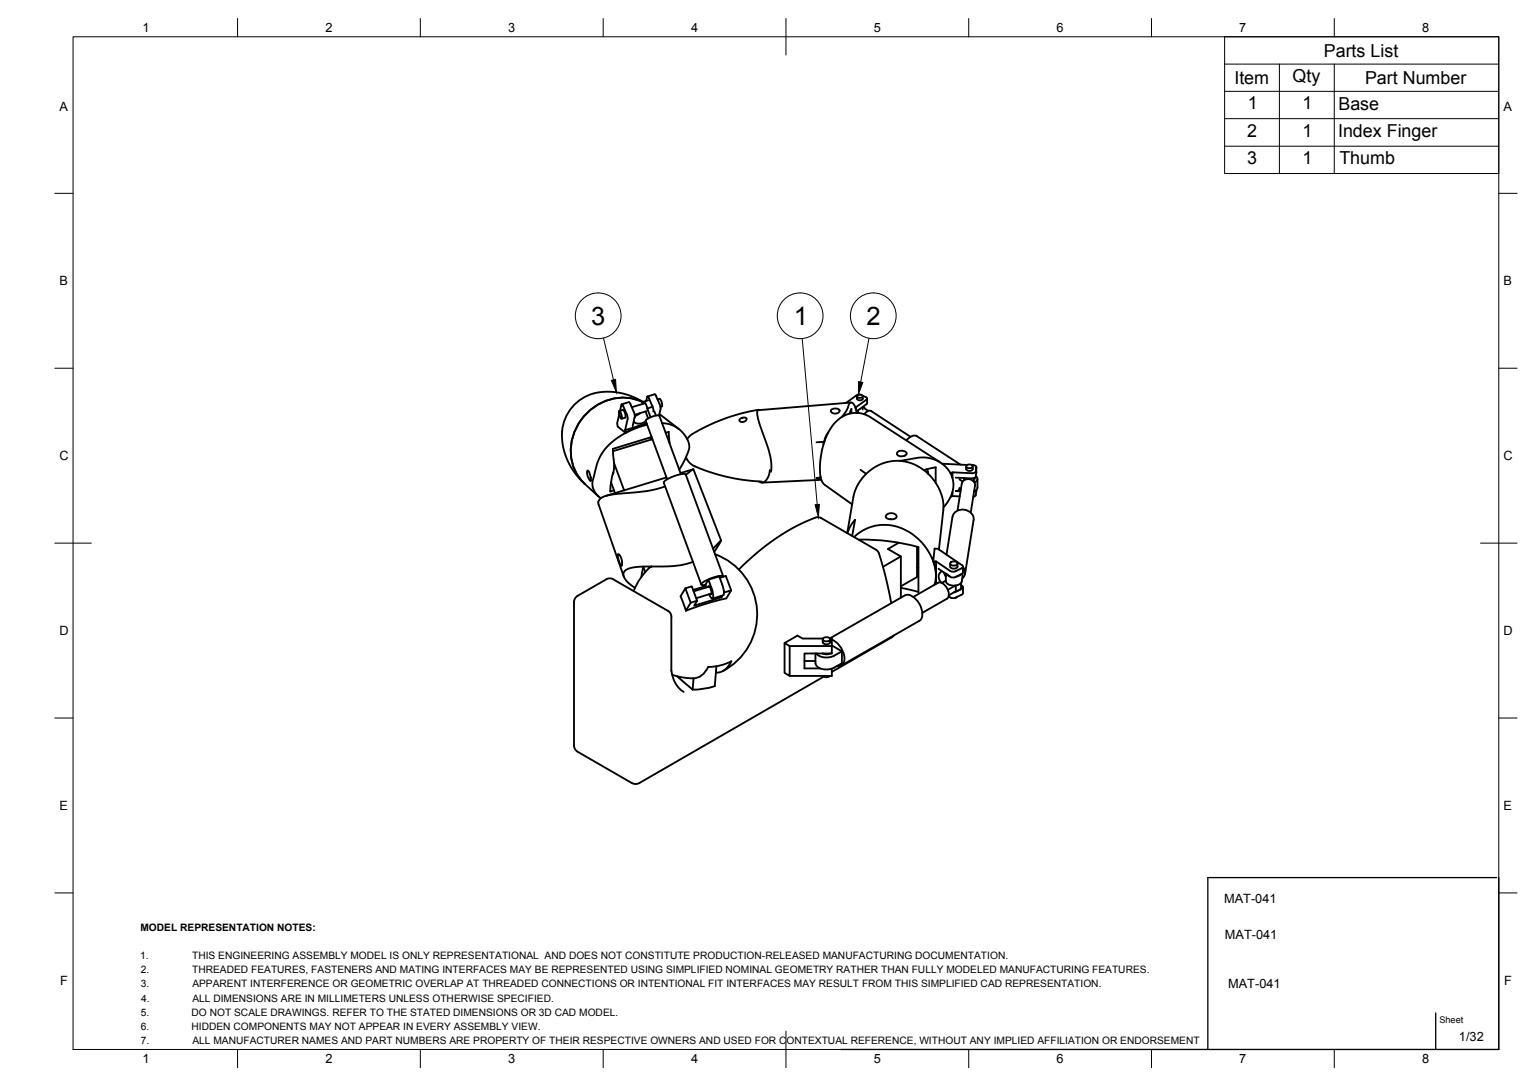
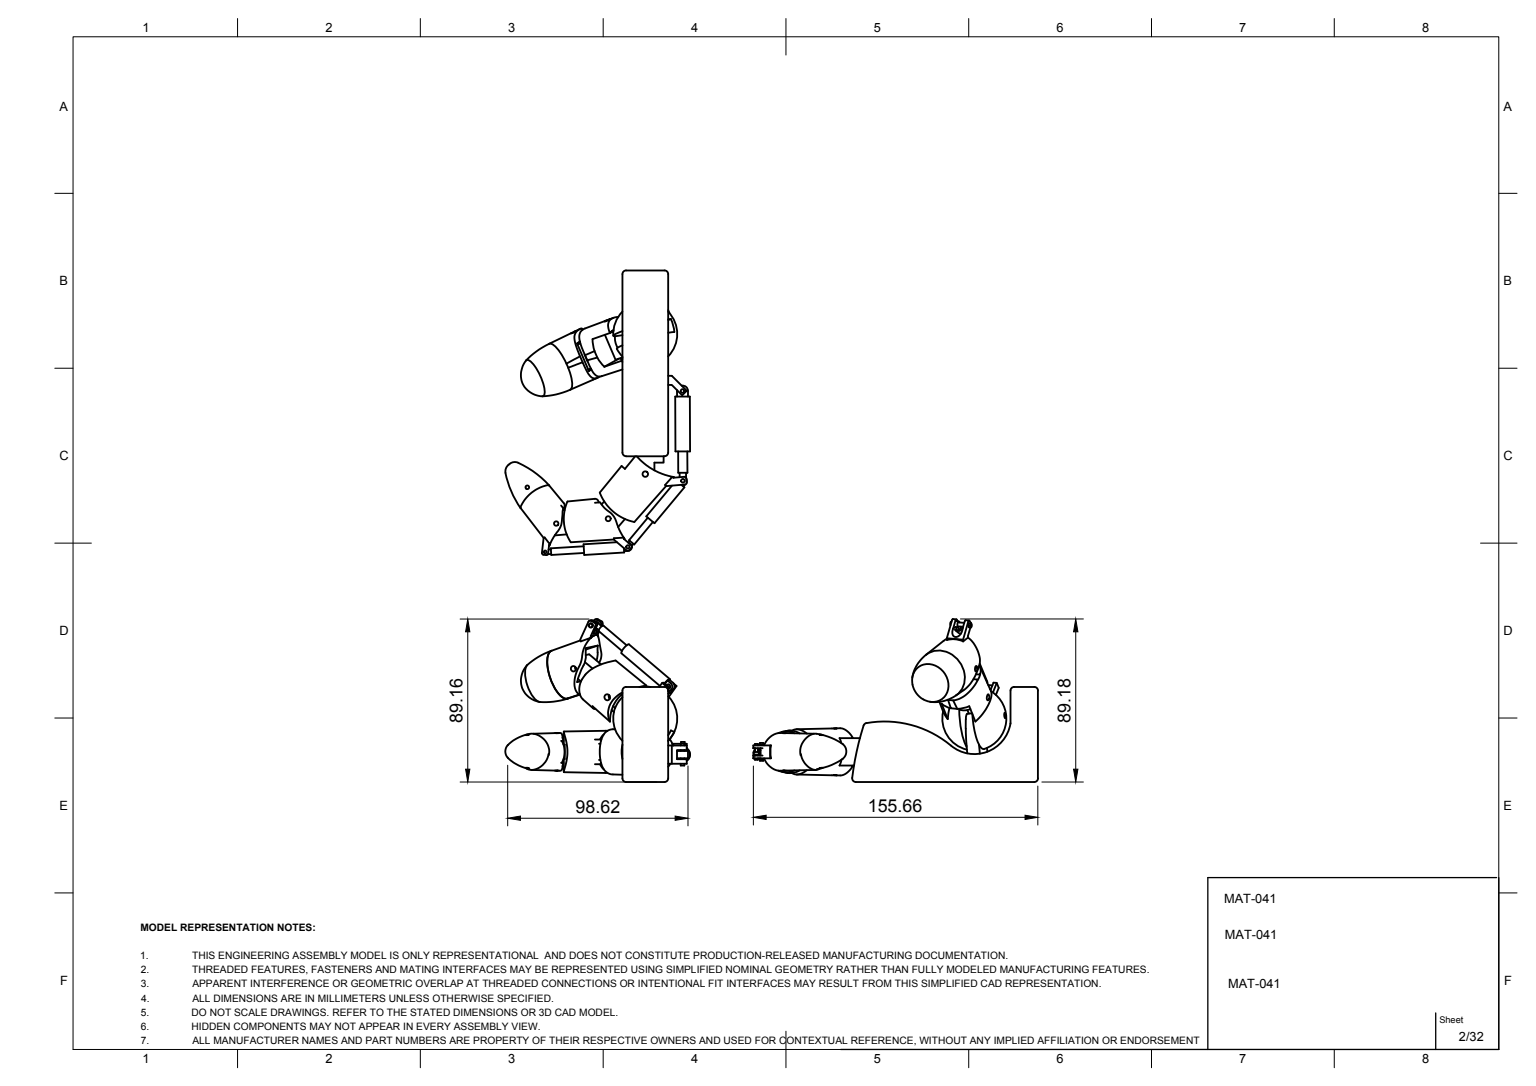
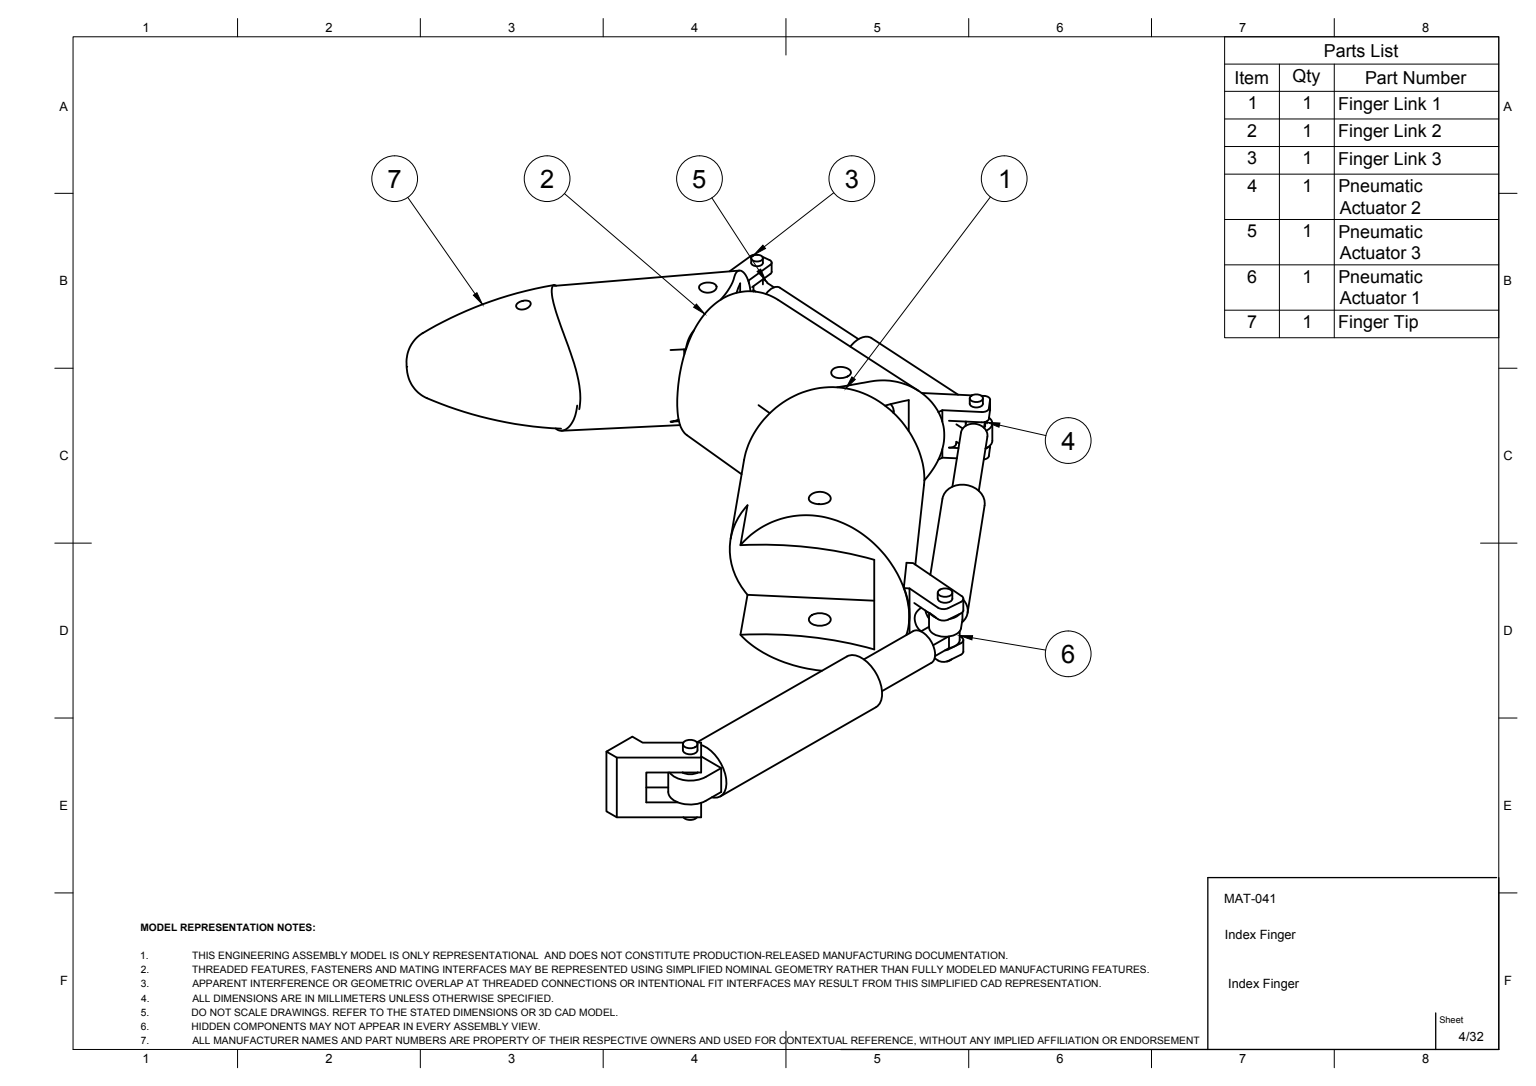
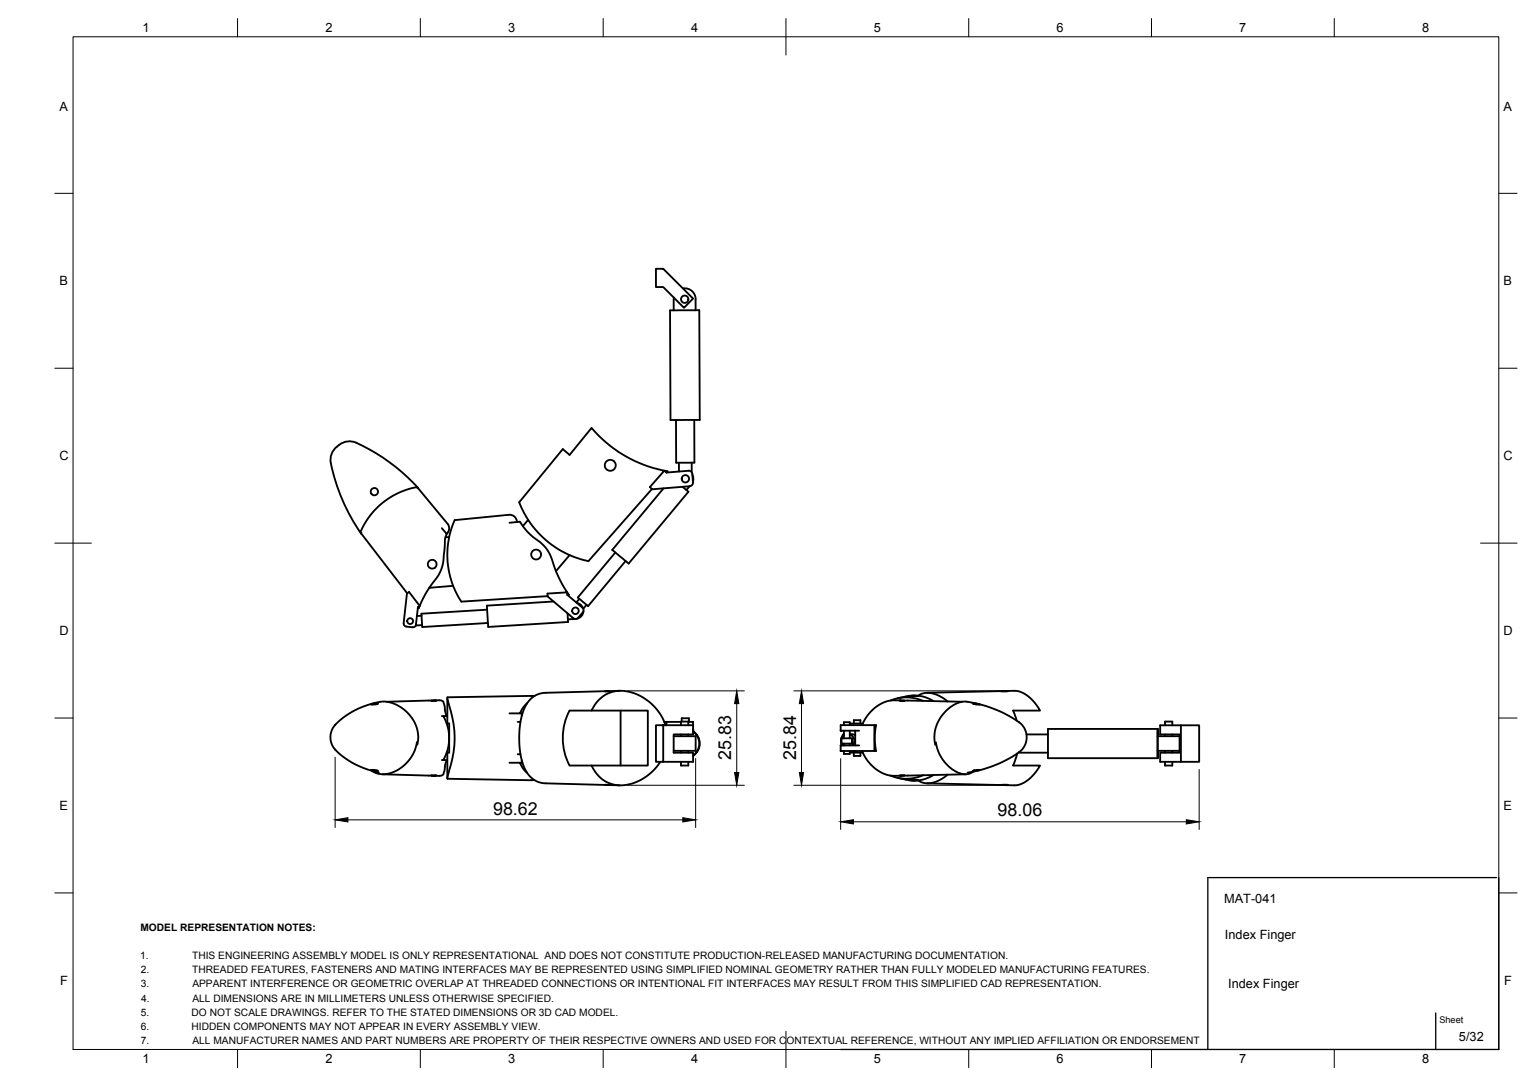
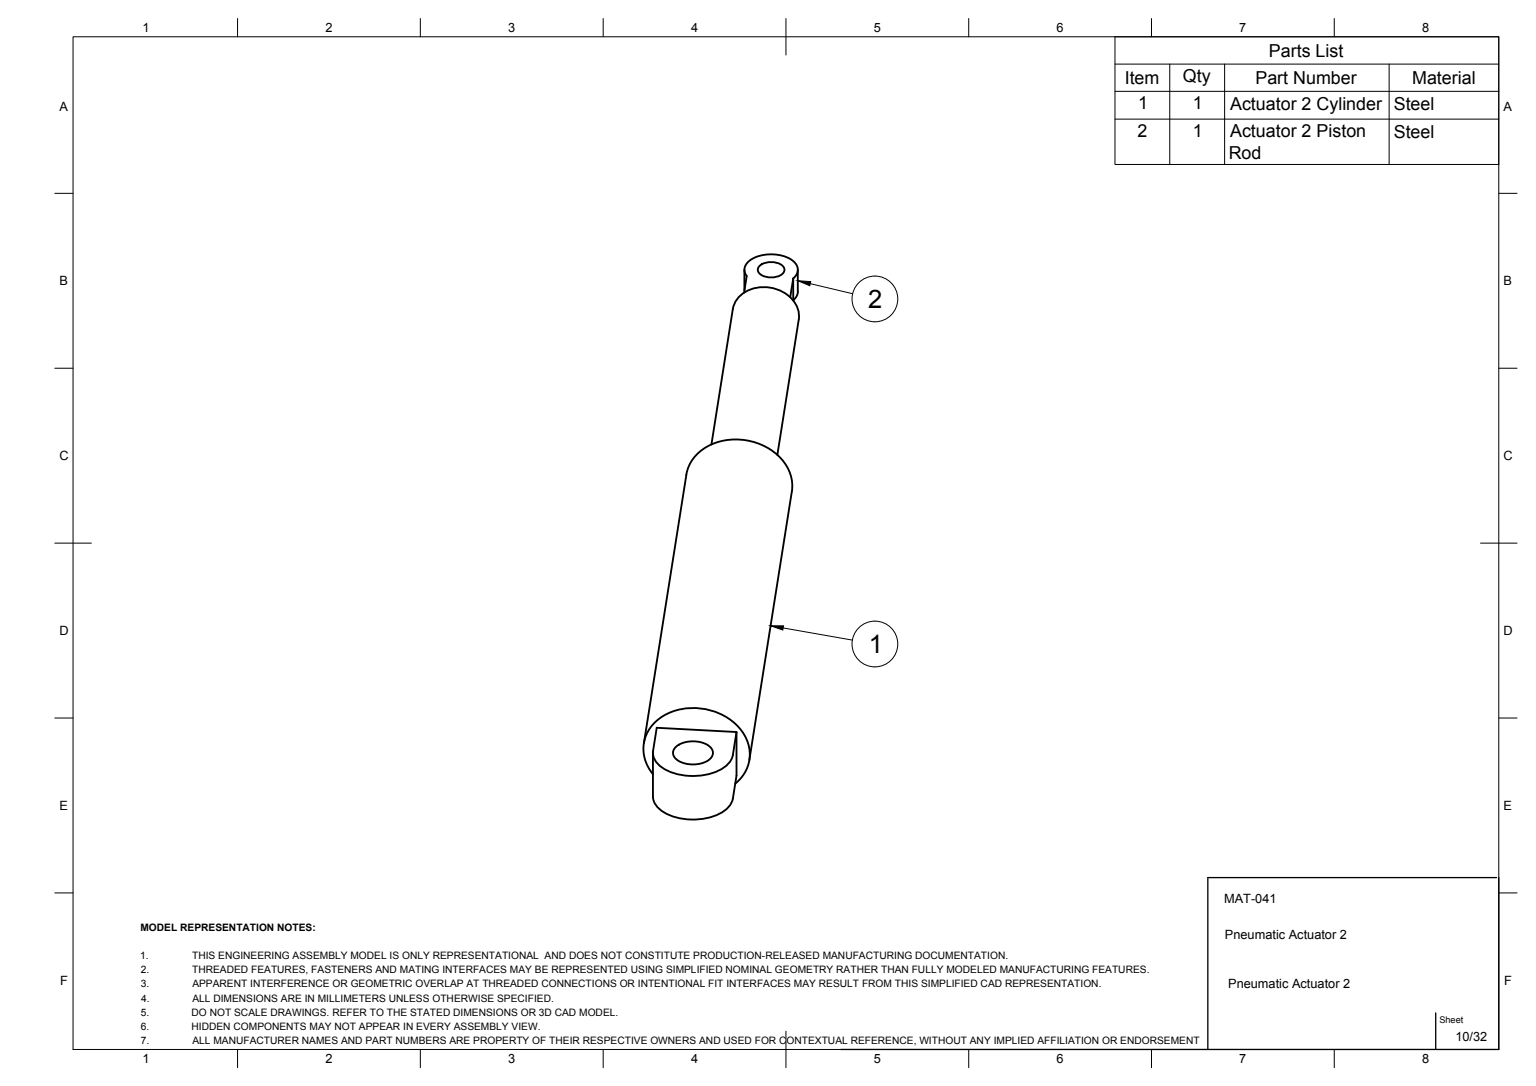
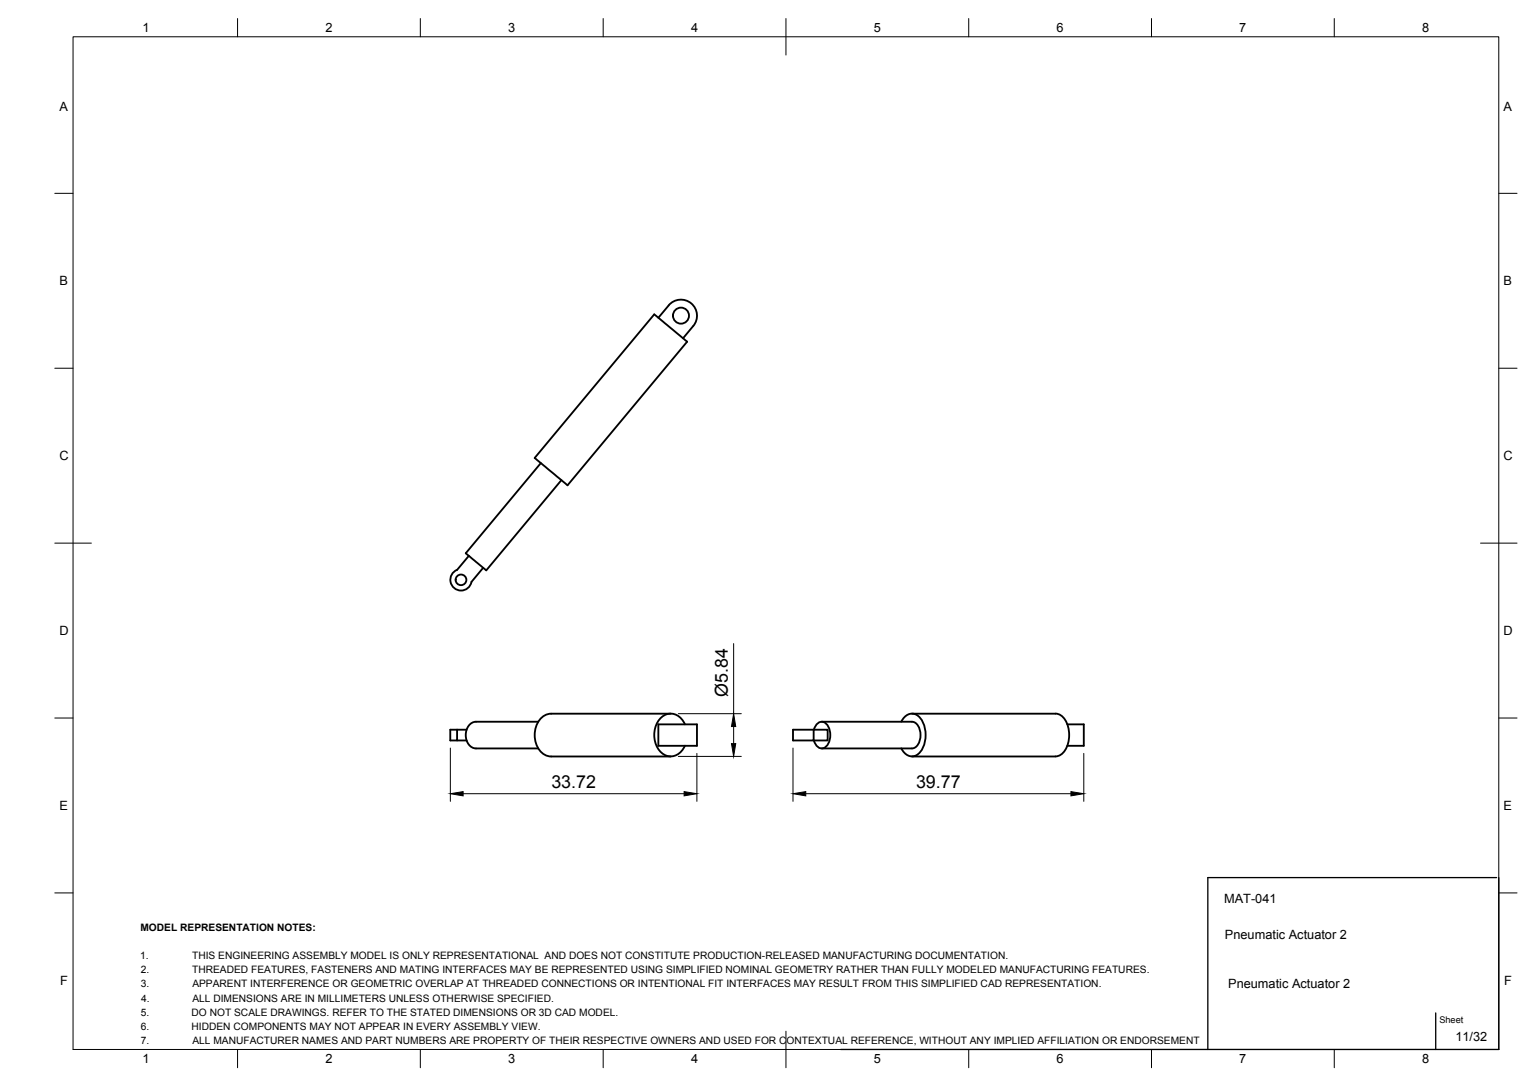
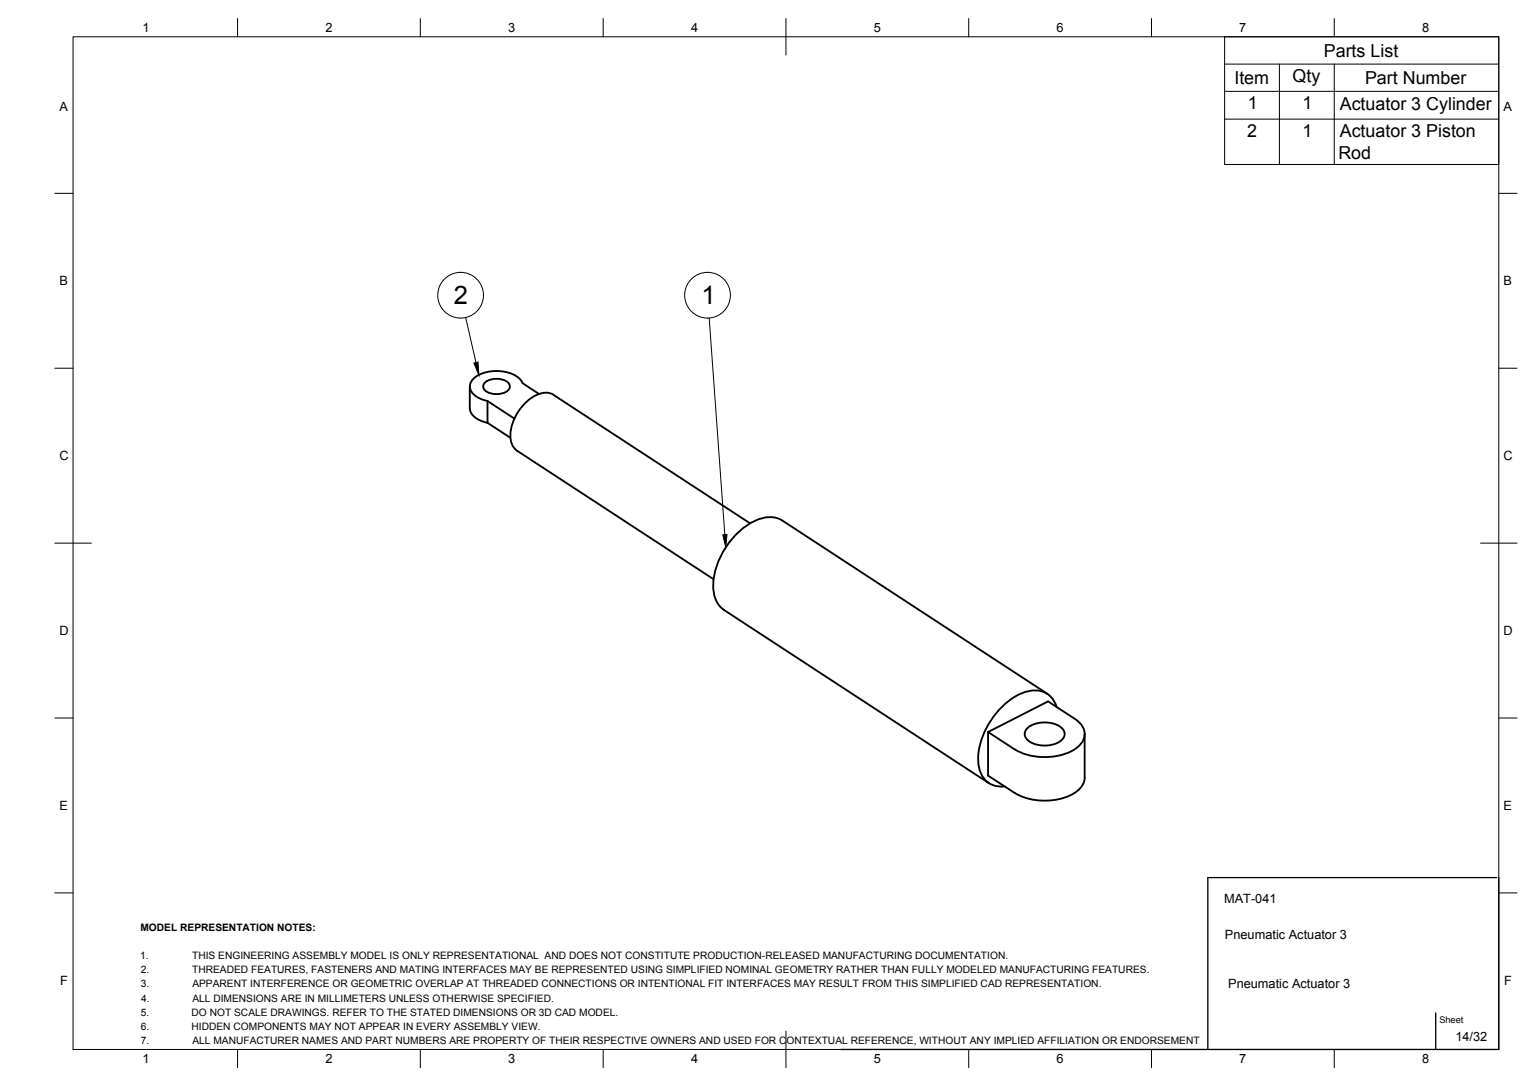
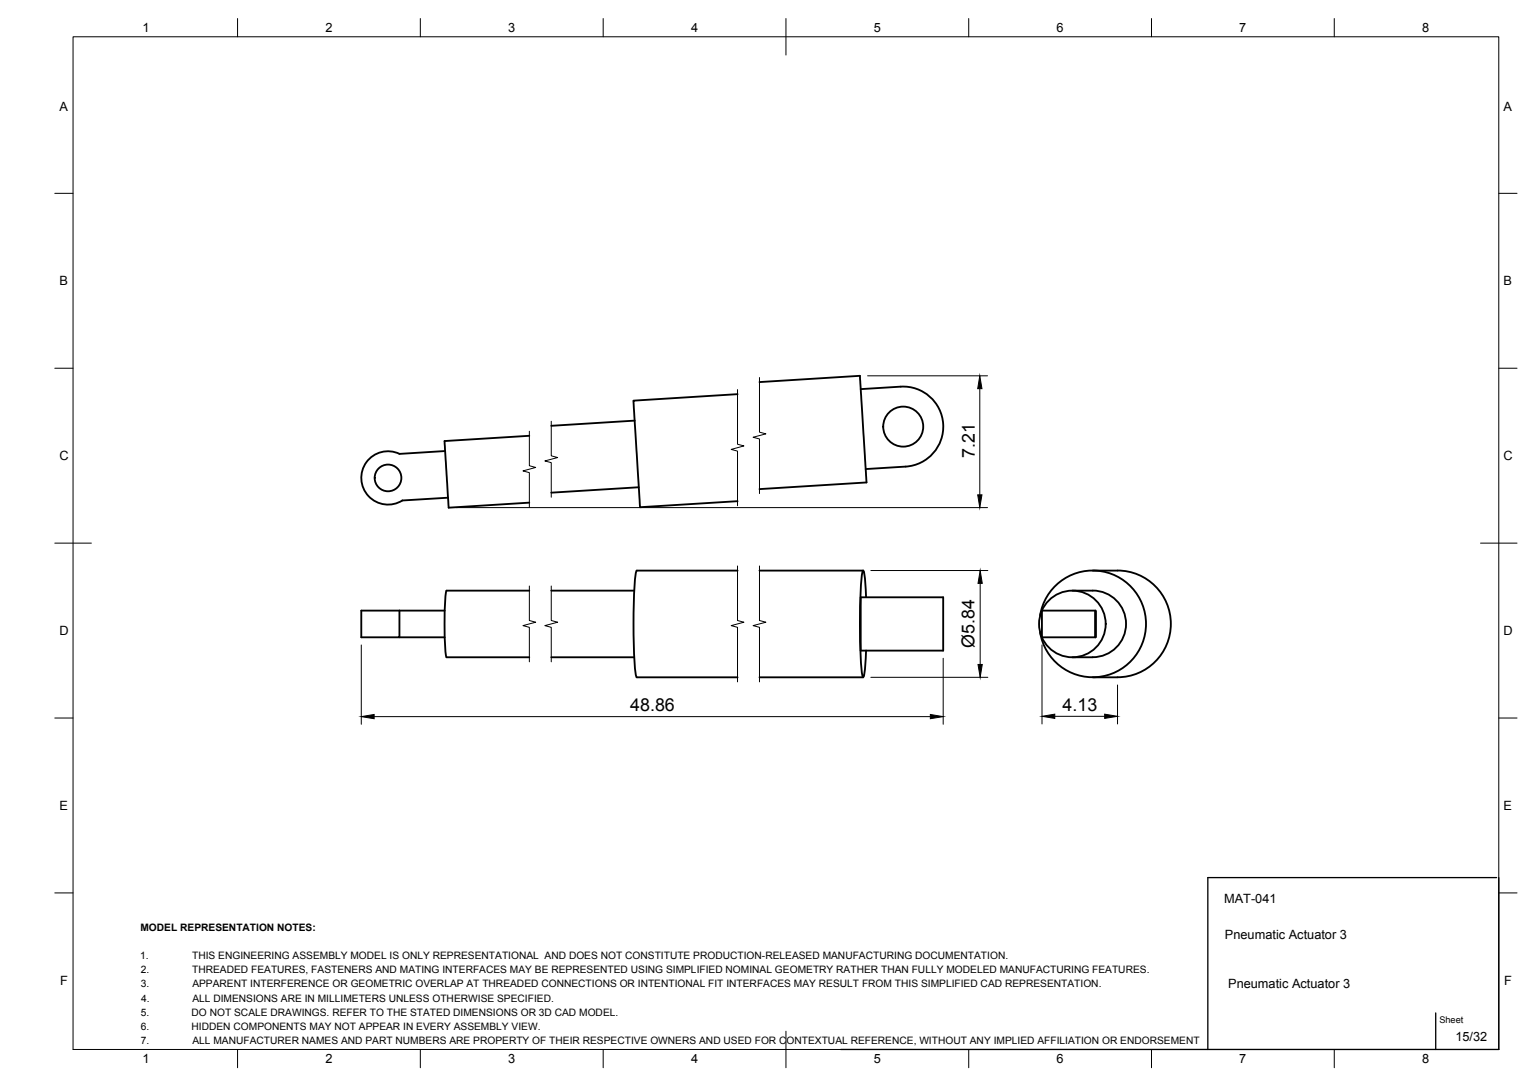
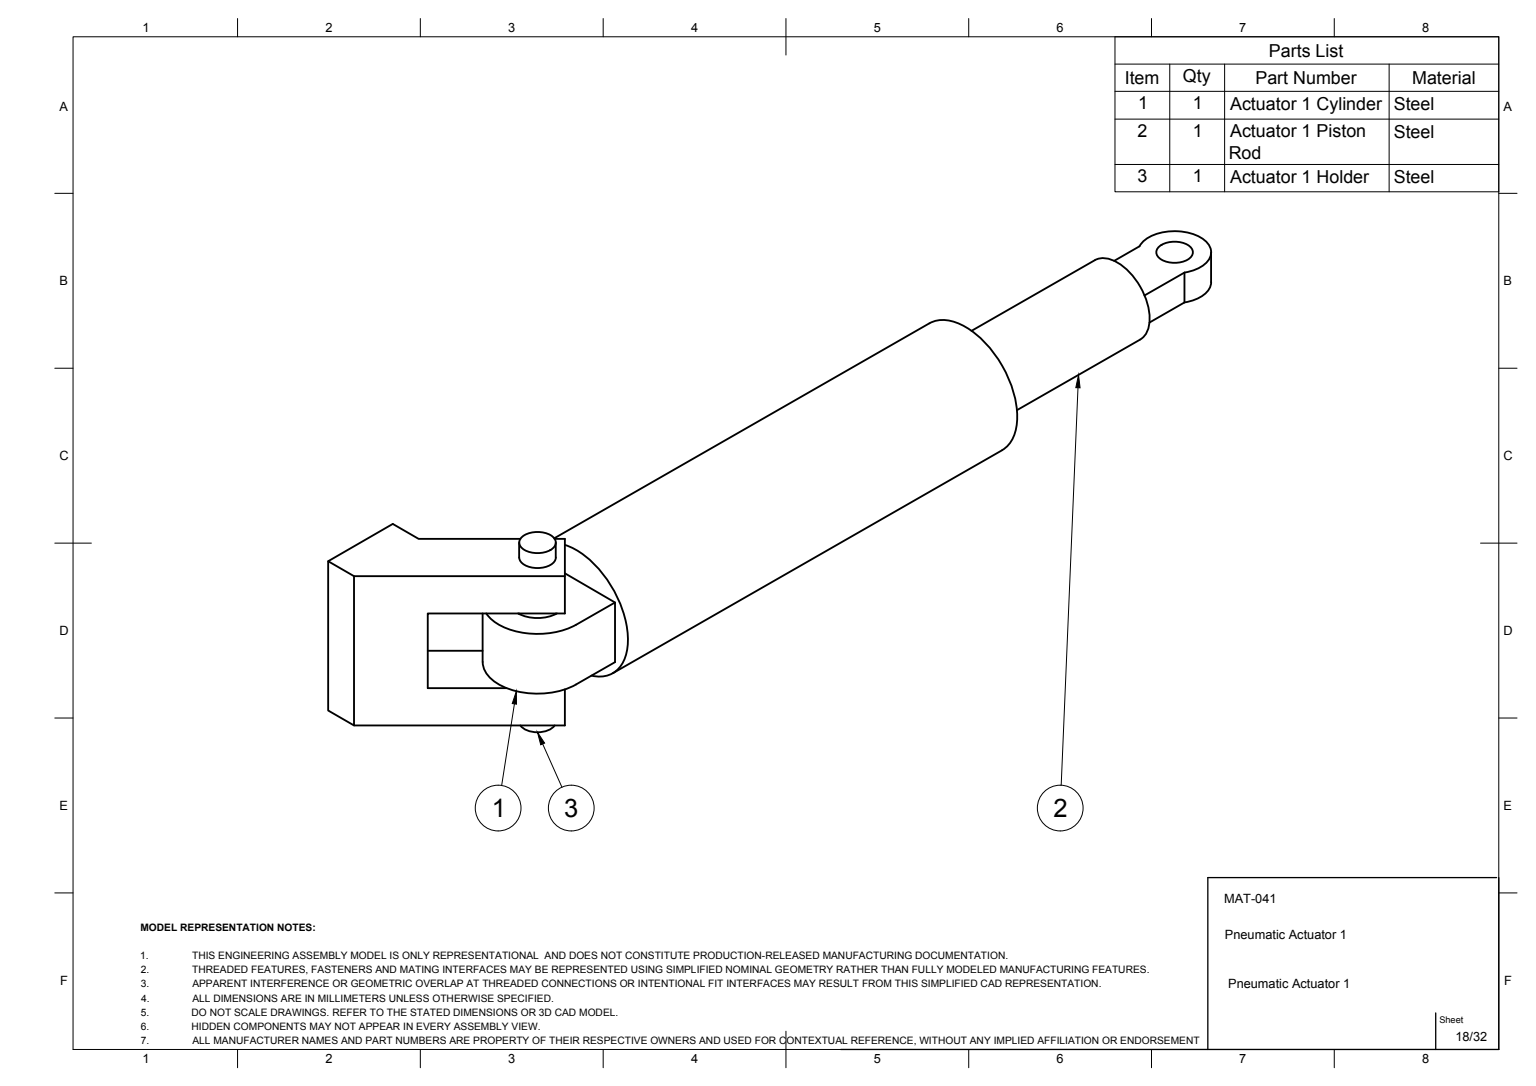
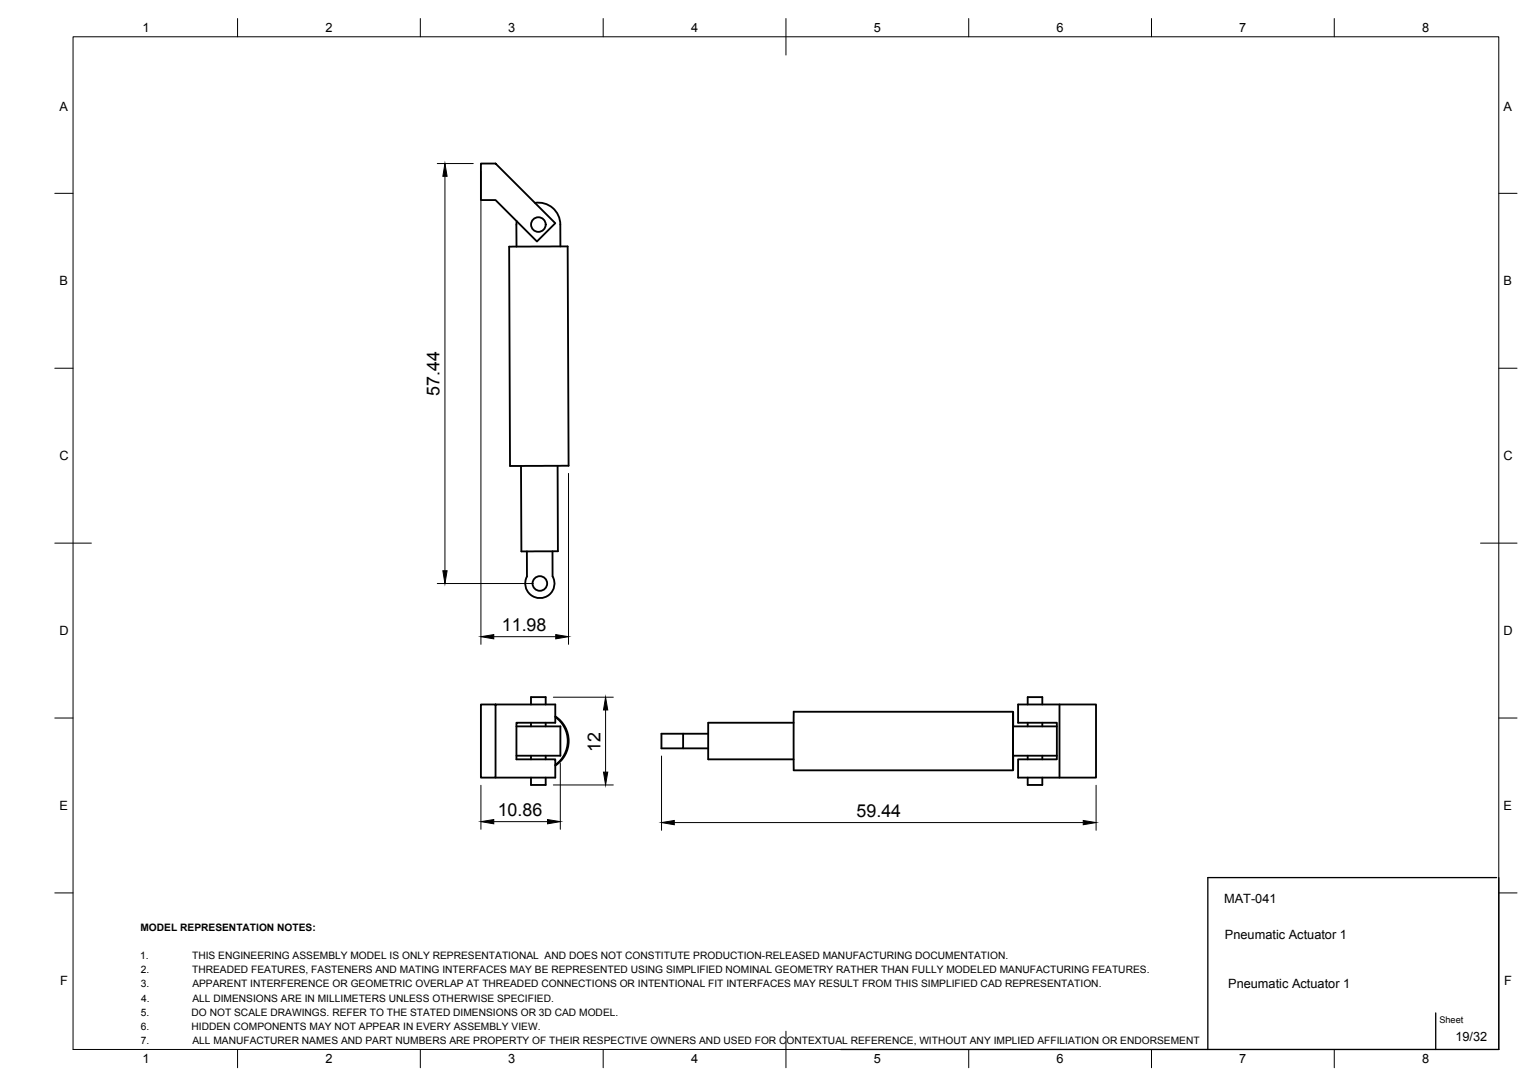
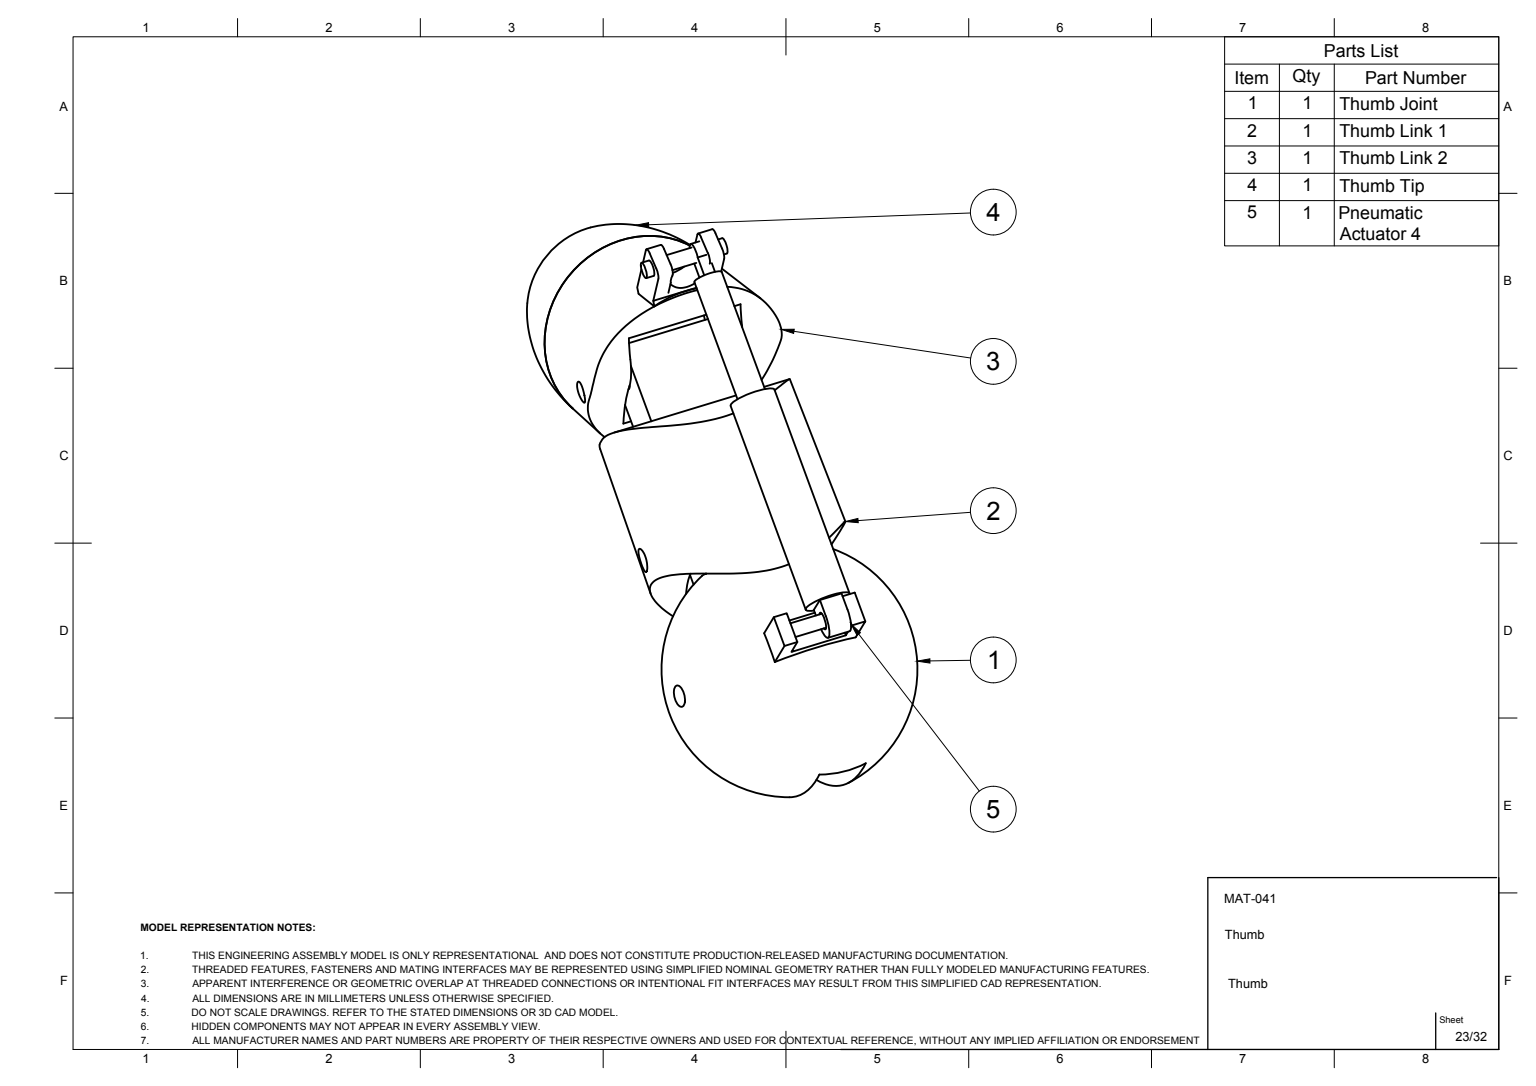
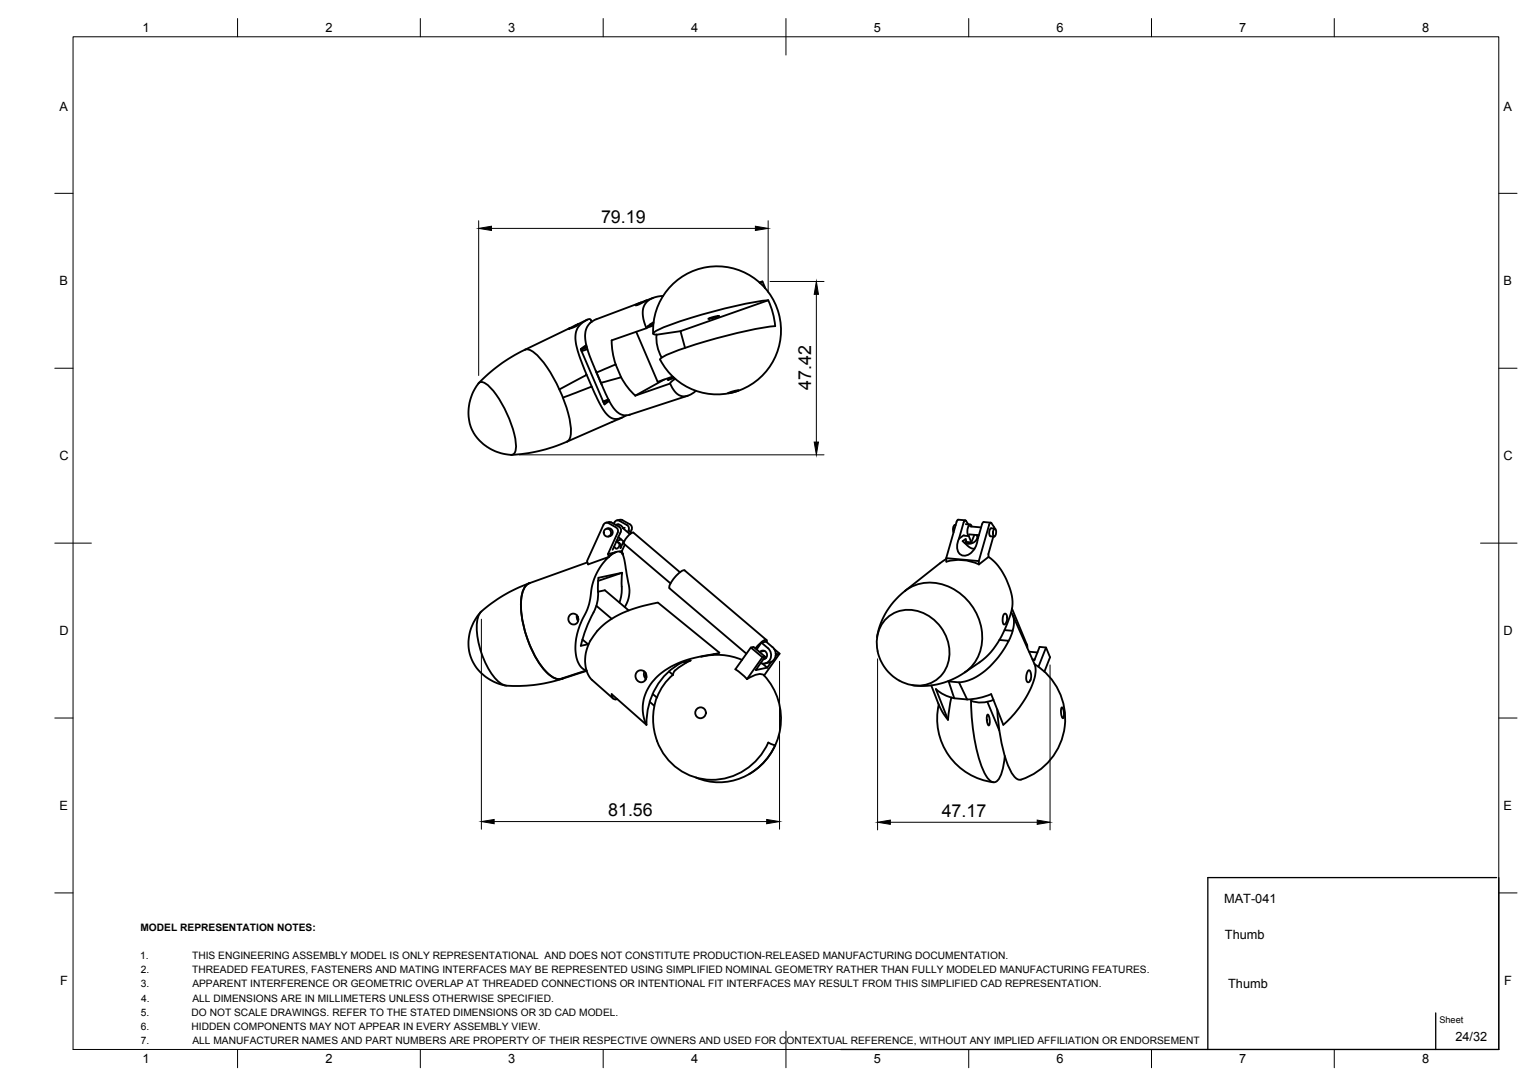
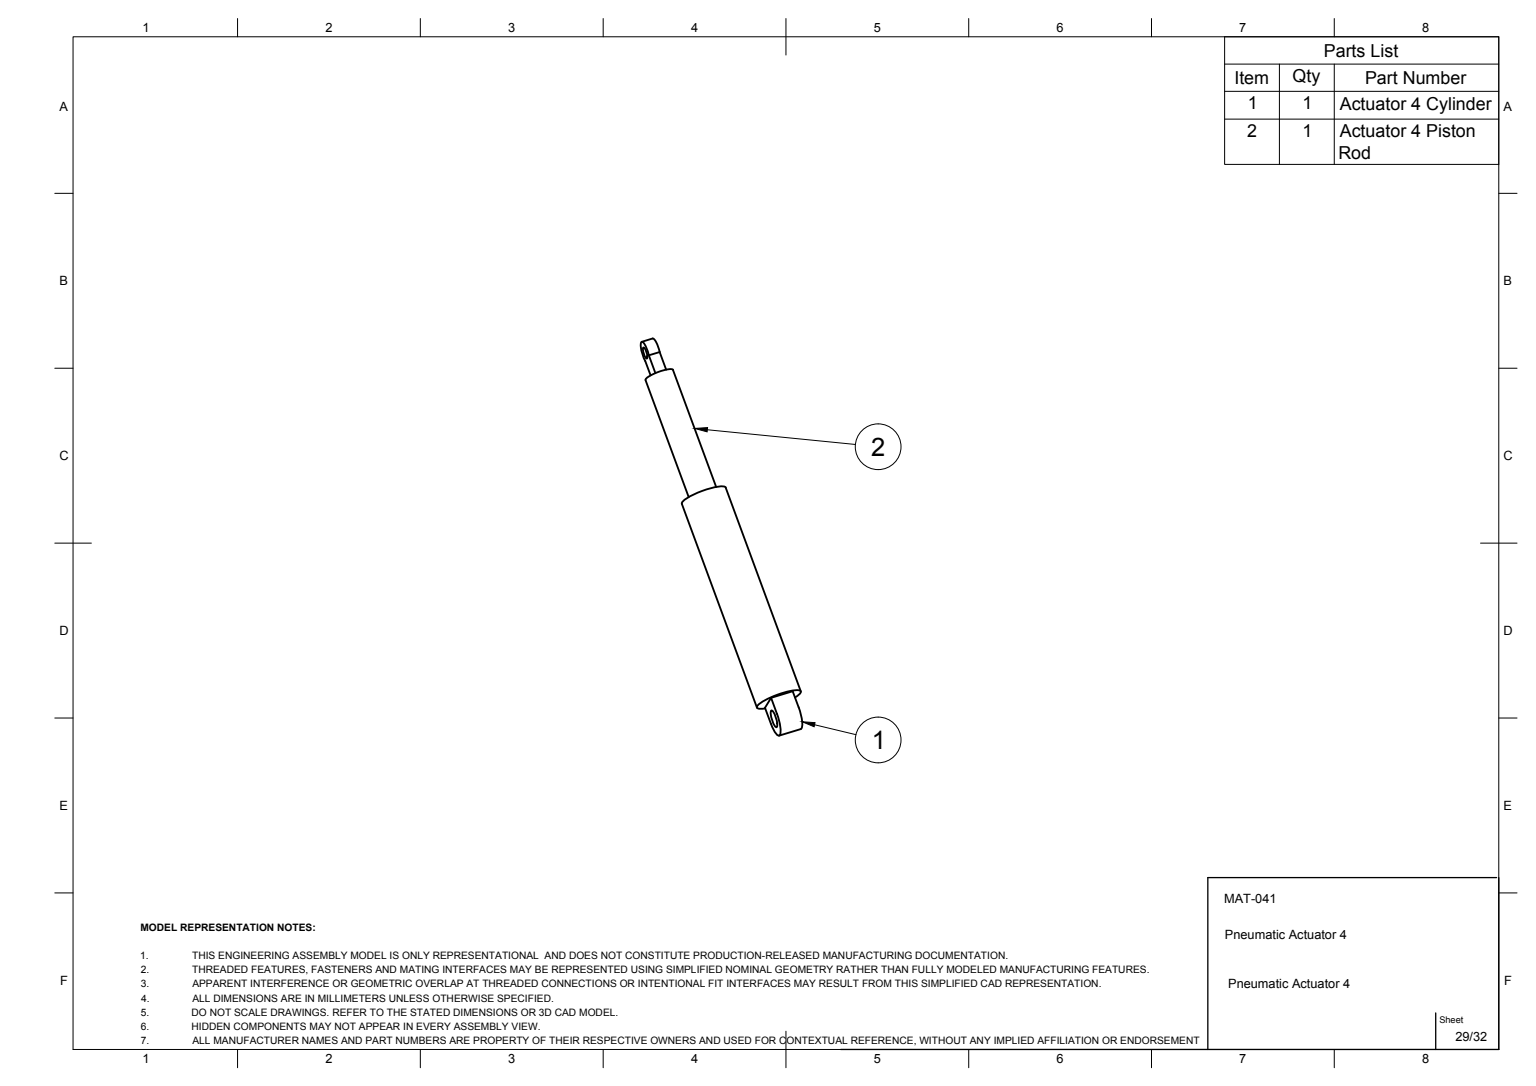
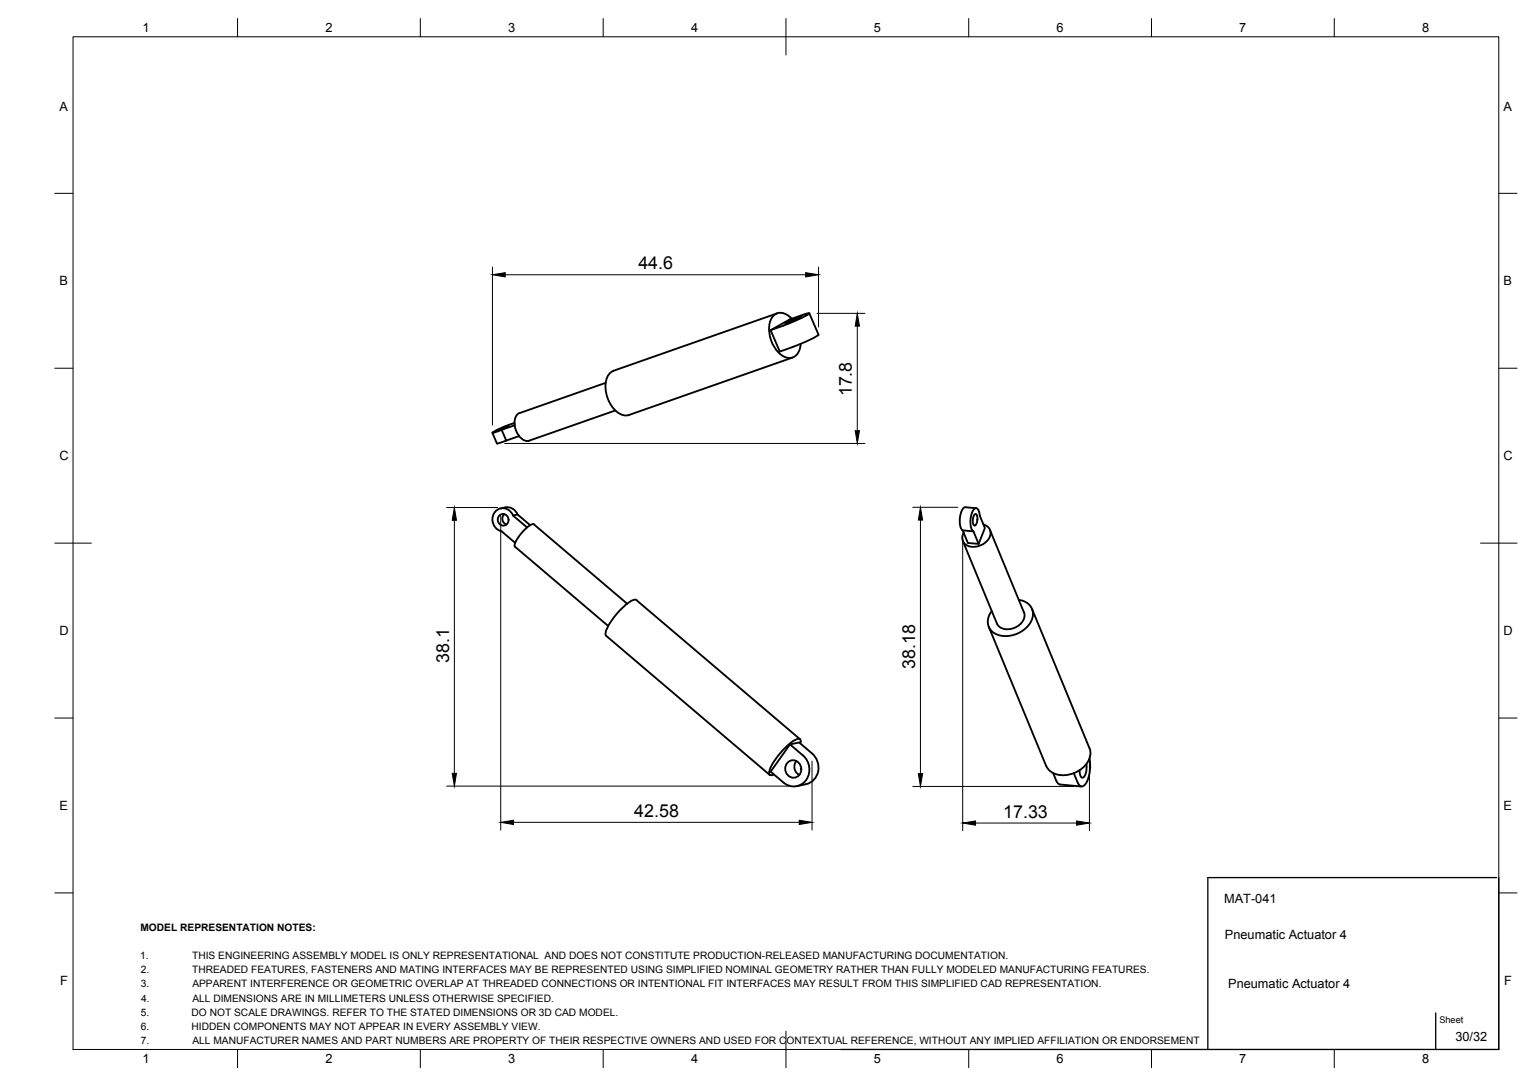
ISO-10303-21;
HEADER;
/* Generated by software containing ST-Developer
 * from STEP Tools, Inc. (www.steptools.com) 
 */

FILE_DESCRIPTION(
/* description */ ('STEP AP214'),
/* implementation_level */ '2;1');

FILE_NAME(
/* name */ 'MAT-041.step',
/* time_stamp */ '2026-11-14T21:57:47-08:00',
/* author */ (''),
/* organization */ (''),
/* preprocessor_version */ 'ST-DEVELOPER v20.2',
/* originating_system */ 'Autodesk Translation Framework v15.17.0.0',
/* authorisation */ '');

FILE_SCHEMA (('AUTOMOTIVE_DESIGN { 1 0 10303 214 3 1 1 }'));
ENDSEC;

DATA;
#10=MECHANICAL_DESIGN_GEOMETRIC_PRESENTATION_REPRESENTATION('',(#248,#249,
#250,#251,#252,#253,#254,#255,#256,#257,#258,#259,#260,#261,#262,#263,#264,
#265),#13199);
#11=(
BOUNDED_CURVE()
B_SPLINE_CURVE(2,(#12139,#12140,#12141),.UNSPECIFIED.,.F.,.F.)
B_SPLINE_CURVE_WITH_KNOTS((3,3),(0.0658194535624849,0.468554524158603),
 .UNSPECIFIED.)
CURVE()
GEOMETRIC_REPRESENTATION_ITEM()
RATIONAL_B_SPLINE_CURVE((0.999935484054137,0.979761934520674,1.))
REPRESENTATION_ITEM('')
);
#12=(
BOUNDED_CURVE()
B_SPLINE_CURVE(2,(#12481,#12482,#12483),.UNSPECIFIED.,.F.,.F.)
B_SPLINE_CURVE_WITH_KNOTS((3,3),(-1.60124615225297,-0.808783730274253),
 .UNSPECIFIED.)
CURVE()
GEOMETRIC_REPRESENTATION_ITEM()
RATIONAL_B_SPLINE_CURVE((1.00284139361103,1.00297035013721,1.00227572336188))
REPRESENTATION_ITEM('')
);
#13=(
BOUNDED_CURVE()
B_SPLINE_CURVE(2,(#12547,#12548,#12549),.UNSPECIFIED.,.F.,.F.)
B_SPLINE_CURVE_WITH_KNOTS((3,3),(-2.14592066681242,-1.35342729440919),
 .UNSPECIFIED.)
CURVE()
GEOMETRIC_REPRESENTATION_ITEM()
RATIONAL_B_SPLINE_CURVE((1.00227603694351,1.00297081766941,1.00284201479666))
REPRESENTATION_ITEM('')
);
#14=(
BOUNDED_CURVE()
B_SPLINE_CURVE(2,(#12779,#12780,#12781),.UNSPECIFIED.,.F.,.F.)
B_SPLINE_CURVE_WITH_KNOTS((3,3),(-2.71364129597392,-1.62020359036119),
 .UNSPECIFIED.)
CURVE()
GEOMETRIC_REPRESENTATION_ITEM()
RATIONAL_B_SPLINE_CURVE((1.0005626059293,1.00242625759818,1.00269667985146))
REPRESENTATION_ITEM('')
);
#15=(
BOUNDED_CURVE()
B_SPLINE_CURVE(2,(#12785,#12786,#12787),.UNSPECIFIED.,.F.,.F.)
B_SPLINE_CURVE_WITH_KNOTS((3,3),(-1.2490205262323,-0.155582820602816),
 .UNSPECIFIED.)
CURVE()
GEOMETRIC_REPRESENTATION_ITEM()
RATIONAL_B_SPLINE_CURVE((1.00269667985147,1.00242625759819,1.00056260592924))
REPRESENTATION_ITEM('')
);
#16=(
BOUNDED_CURVE()
B_SPLINE_CURVE(2,(#12826,#12827,#12828),.UNSPECIFIED.,.F.,.F.)
B_SPLINE_CURVE_WITH_KNOTS((3,3),(0.587541837462245,1.2406747936684),
 .UNSPECIFIED.)
CURVE()
GEOMETRIC_REPRESENTATION_ITEM()
RATIONAL_B_SPLINE_CURVE((1.00007054095476,1.00010145473128,1.00011392829506))
REPRESENTATION_ITEM('')
);
#17=(
BOUNDED_SURFACE()
B_SPLINE_SURFACE(2,2,((#12039,#12040,#12041,#12042,#12043,#12044,#12045,
#12046,#12047),(#12048,#12049,#12050,#12051,#12052,#12053,#12054,#12055,
#12056),(#12057,#12058,#12059,#12060,#12061,#12062,#12063,#12064,#12065)),
 .UNSPECIFIED.,.F.,.T.,.F.)
B_SPLINE_SURFACE_WITH_KNOTS((3,3),(3,2,2,2,3),(-1.66348996389916,-0.482485072527983),
(-3.14159265358979,-1.5707963267949,0.,1.5707963267949,3.14159265358979),
 .UNSPECIFIED.)
GEOMETRIC_REPRESENTATION_ITEM()
RATIONAL_B_SPLINE_SURFACE(((1.,0.707106781186548,1.,0.707106781186548,1.,
0.707106781186548,1.,0.707106781186548,1.),(0.830661033030149,0.587366049323041,
0.830661033030149,0.587366049323041,0.830661033030149,0.587366049323041,
0.830661033030149,0.587366049323041,0.830661033030149),(1.,0.707106781186548,
1.,0.707106781186548,1.,0.707106781186548,1.,0.707106781186548,1.)))
REPRESENTATION_ITEM('')
SURFACE()
);
#18=(
BOUNDED_SURFACE()
B_SPLINE_SURFACE(2,2,((#12070,#12071,#12072,#12073,#12074,#12075,#12076,
#12077,#12078),(#12079,#12080,#12081,#12082,#12083,#12084,#12085,#12086,
#12087),(#12088,#12089,#12090,#12091,#12092,#12093,#12094,#12095,#12096)),
 .UNSPECIFIED.,.F.,.T.,.F.)
B_SPLINE_SURFACE_WITH_KNOTS((3,3),(3,2,2,2,3),(-0.468554524158603,-0.0651764989564067),
(-3.14159265358979,-1.5707963267949,0.,1.5707963267949,3.14159265358979),
 .UNSPECIFIED.)
GEOMETRIC_REPRESENTATION_ITEM()
RATIONAL_B_SPLINE_SURFACE(((1.,0.707106781186548,1.,0.707106781186548,1.,
0.707106781186548,1.,0.707106781186548,1.),(0.979729625048845,0.692773461601392,
0.979729625048845,0.692773461601392,0.979729625048845,0.692773461601392,
0.979729625048845,0.692773461601392,0.979729625048845),(1.,0.707106781186548,
1.,0.707106781186548,1.,0.707106781186548,1.,0.707106781186548,1.)))
REPRESENTATION_ITEM('')
SURFACE()
);
#19=(
BOUNDED_SURFACE()
B_SPLINE_SURFACE(2,2,((#12988,#12989,#12990,#12991,#12992,#12993,#12994,
#12995,#12996),(#12997,#12998,#12999,#13000,#13001,#13002,#13003,#13004,
#13005),(#13006,#13007,#13008,#13009,#13010,#13011,#13012,#13013,#13014)),
 .UNSPECIFIED.,.F.,.T.,.F.)
B_SPLINE_SURFACE_WITH_KNOTS((3,3),(3,2,2,2,3),(-1.48074001480244,-0.468405301545521),
(-3.14159265358979,-1.5707963267949,0.,1.5707963267949,3.14159265358979),
 .UNSPECIFIED.)
GEOMETRIC_REPRESENTATION_ITEM()
RATIONAL_B_SPLINE_SURFACE(((1.,0.707106781186548,1.,0.707106781186548,1.,
0.707106781186548,1.,0.707106781186548,1.),(0.874609102422644,0.618442027210531,
0.874609102422644,0.618442027210531,0.874609102422644,0.618442027210531,
0.874609102422644,0.618442027210531,0.874609102422644),(1.,0.707106781186548,
1.,0.707106781186548,1.,0.707106781186548,1.,0.707106781186548,1.)))
REPRESENTATION_ITEM('')
SURFACE()
);
#20=(
BOUNDED_SURFACE()
B_SPLINE_SURFACE(2,2,((#13019,#13020,#13021,#13022,#13023,#13024,#13025,
#13026,#13027),(#13028,#13029,#13030,#13031,#13032,#13033,#13034,#13035,
#13036),(#13037,#13038,#13039,#13040,#13041,#13042,#13043,#13044,#13045)),
 .UNSPECIFIED.,.F.,.T.,.F.)
B_SPLINE_SURFACE_WITH_KNOTS((3,3),(3,2,2,2,3),(-0.359971068140638,-0.0153537783592699),
(-3.14159265358979,-1.5707963267949,0.,1.5707963267949,3.14159265358979),
 .UNSPECIFIED.)
GEOMETRIC_REPRESENTATION_ITEM()
RATIONAL_B_SPLINE_SURFACE(((1.,0.707106781186548,1.,0.707106781186548,1.,
0.707106781186548,1.,0.707106781186548,1.),(0.985191558786762,0.696635631985865,
0.985191558786762,0.696635631985865,0.985191558786762,0.696635631985865,
0.985191558786762,0.696635631985865,0.985191558786762),(1.,0.707106781186548,
1.,0.707106781186548,1.,0.707106781186548,1.,0.707106781186548,1.)))
REPRESENTATION_ITEM('')
SURFACE()
);
#21=ITEM_DEFINED_TRANSFORMATION($,$,#7454,#7490);
#22=ITEM_DEFINED_TRANSFORMATION($,$,#7474,#7491);
#23=ITEM_DEFINED_TRANSFORMATION($,$,#7493,#7529);
#24=ITEM_DEFINED_TRANSFORMATION($,$,#7513,#7530);
#25=ITEM_DEFINED_TRANSFORMATION($,$,#7532,#7592);
#26=ITEM_DEFINED_TRANSFORMATION($,$,#7552,#7593);
#27=ITEM_DEFINED_TRANSFORMATION($,$,#7568,#7594);
#28=ITEM_DEFINED_TRANSFORMATION($,$,#7193,#7610);
#29=ITEM_DEFINED_TRANSFORMATION($,$,#7274,#7611);
#30=ITEM_DEFINED_TRANSFORMATION($,$,#7359,#7612);
#31=ITEM_DEFINED_TRANSFORMATION($,$,#7453,#7613);
#32=ITEM_DEFINED_TRANSFORMATION($,$,#7492,#7614);
#33=ITEM_DEFINED_TRANSFORMATION($,$,#7531,#7615);
#34=ITEM_DEFINED_TRANSFORMATION($,$,#7595,#7616);
#35=ITEM_DEFINED_TRANSFORMATION($,$,#7783,#7819);
#36=ITEM_DEFINED_TRANSFORMATION($,$,#7803,#7820);
#37=ITEM_DEFINED_TRANSFORMATION($,$,#7618,#7821);
#38=ITEM_DEFINED_TRANSFORMATION($,$,#7666,#7822);
#39=ITEM_DEFINED_TRANSFORMATION($,$,#7700,#7823);
#40=ITEM_DEFINED_TRANSFORMATION($,$,#7776,#7824);
#41=ITEM_DEFINED_TRANSFORMATION($,$,#7782,#7825);
#42=ITEM_DEFINED_TRANSFORMATION($,$,#7061,#7826);
#43=ITEM_DEFINED_TRANSFORMATION($,$,#7192,#7827);
#44=ITEM_DEFINED_TRANSFORMATION($,$,#7617,#7828);
#45=(
REPRESENTATION_RELATIONSHIP($,$,#13285,#13284)
REPRESENTATION_RELATIONSHIP_WITH_TRANSFORMATION(#21)
SHAPE_REPRESENTATION_RELATIONSHIP()
);
#46=(
REPRESENTATION_RELATIONSHIP($,$,#13286,#13284)
REPRESENTATION_RELATIONSHIP_WITH_TRANSFORMATION(#22)
SHAPE_REPRESENTATION_RELATIONSHIP()
);
#47=(
REPRESENTATION_RELATIONSHIP($,$,#13288,#13287)
REPRESENTATION_RELATIONSHIP_WITH_TRANSFORMATION(#23)
SHAPE_REPRESENTATION_RELATIONSHIP()
);
#48=(
REPRESENTATION_RELATIONSHIP($,$,#13289,#13287)
REPRESENTATION_RELATIONSHIP_WITH_TRANSFORMATION(#24)
SHAPE_REPRESENTATION_RELATIONSHIP()
);
#49=(
REPRESENTATION_RELATIONSHIP($,$,#13291,#13290)
REPRESENTATION_RELATIONSHIP_WITH_TRANSFORMATION(#25)
SHAPE_REPRESENTATION_RELATIONSHIP()
);
#50=(
REPRESENTATION_RELATIONSHIP($,$,#13292,#13290)
REPRESENTATION_RELATIONSHIP_WITH_TRANSFORMATION(#26)
SHAPE_REPRESENTATION_RELATIONSHIP()
);
#51=(
REPRESENTATION_RELATIONSHIP($,$,#13293,#13290)
REPRESENTATION_RELATIONSHIP_WITH_TRANSFORMATION(#27)
SHAPE_REPRESENTATION_RELATIONSHIP()
);
#52=(
REPRESENTATION_RELATIONSHIP($,$,#13281,#13280)
REPRESENTATION_RELATIONSHIP_WITH_TRANSFORMATION(#28)
SHAPE_REPRESENTATION_RELATIONSHIP()
);
#53=(
REPRESENTATION_RELATIONSHIP($,$,#13282,#13280)
REPRESENTATION_RELATIONSHIP_WITH_TRANSFORMATION(#29)
SHAPE_REPRESENTATION_RELATIONSHIP()
);
#54=(
REPRESENTATION_RELATIONSHIP($,$,#13283,#13280)
REPRESENTATION_RELATIONSHIP_WITH_TRANSFORMATION(#30)
SHAPE_REPRESENTATION_RELATIONSHIP()
);
#55=(
REPRESENTATION_RELATIONSHIP($,$,#13284,#13280)
REPRESENTATION_RELATIONSHIP_WITH_TRANSFORMATION(#31)
SHAPE_REPRESENTATION_RELATIONSHIP()
);
#56=(
REPRESENTATION_RELATIONSHIP($,$,#13287,#13280)
REPRESENTATION_RELATIONSHIP_WITH_TRANSFORMATION(#32)
SHAPE_REPRESENTATION_RELATIONSHIP()
);
#57=(
REPRESENTATION_RELATIONSHIP($,$,#13290,#13280)
REPRESENTATION_RELATIONSHIP_WITH_TRANSFORMATION(#33)
SHAPE_REPRESENTATION_RELATIONSHIP()
);
#58=(
REPRESENTATION_RELATIONSHIP($,$,#13294,#13280)
REPRESENTATION_RELATIONSHIP_WITH_TRANSFORMATION(#34)
SHAPE_REPRESENTATION_RELATIONSHIP()
);
#59=(
REPRESENTATION_RELATIONSHIP($,$,#13301,#13300)
REPRESENTATION_RELATIONSHIP_WITH_TRANSFORMATION(#35)
SHAPE_REPRESENTATION_RELATIONSHIP()
);
#60=(
REPRESENTATION_RELATIONSHIP($,$,#13302,#13300)
REPRESENTATION_RELATIONSHIP_WITH_TRANSFORMATION(#36)
SHAPE_REPRESENTATION_RELATIONSHIP()
);
#61=(
REPRESENTATION_RELATIONSHIP($,$,#13296,#13295)
REPRESENTATION_RELATIONSHIP_WITH_TRANSFORMATION(#37)
SHAPE_REPRESENTATION_RELATIONSHIP()
);
#62=(
REPRESENTATION_RELATIONSHIP($,$,#13297,#13295)
REPRESENTATION_RELATIONSHIP_WITH_TRANSFORMATION(#38)
SHAPE_REPRESENTATION_RELATIONSHIP()
);
#63=(
REPRESENTATION_RELATIONSHIP($,$,#13298,#13295)
REPRESENTATION_RELATIONSHIP_WITH_TRANSFORMATION(#39)
SHAPE_REPRESENTATION_RELATIONSHIP()
);
#64=(
REPRESENTATION_RELATIONSHIP($,$,#13299,#13295)
REPRESENTATION_RELATIONSHIP_WITH_TRANSFORMATION(#40)
SHAPE_REPRESENTATION_RELATIONSHIP()
);
#65=(
REPRESENTATION_RELATIONSHIP($,$,#13300,#13295)
REPRESENTATION_RELATIONSHIP_WITH_TRANSFORMATION(#41)
SHAPE_REPRESENTATION_RELATIONSHIP()
);
#66=(
REPRESENTATION_RELATIONSHIP($,$,#13279,#13278)
REPRESENTATION_RELATIONSHIP_WITH_TRANSFORMATION(#42)
SHAPE_REPRESENTATION_RELATIONSHIP()
);
#67=(
REPRESENTATION_RELATIONSHIP($,$,#13280,#13278)
REPRESENTATION_RELATIONSHIP_WITH_TRANSFORMATION(#43)
SHAPE_REPRESENTATION_RELATIONSHIP()
);
#68=(
REPRESENTATION_RELATIONSHIP($,$,#13295,#13278)
REPRESENTATION_RELATIONSHIP_WITH_TRANSFORMATION(#44)
SHAPE_REPRESENTATION_RELATIONSHIP()
);
#69=CONTEXT_DEPENDENT_SHAPE_REPRESENTATION(#45,#13238);
#70=CONTEXT_DEPENDENT_SHAPE_REPRESENTATION(#46,#13239);
#71=CONTEXT_DEPENDENT_SHAPE_REPRESENTATION(#47,#13243);
#72=CONTEXT_DEPENDENT_SHAPE_REPRESENTATION(#48,#13244);
#73=CONTEXT_DEPENDENT_SHAPE_REPRESENTATION(#49,#13249);
#74=CONTEXT_DEPENDENT_SHAPE_REPRESENTATION(#50,#13250);
#75=CONTEXT_DEPENDENT_SHAPE_REPRESENTATION(#51,#13251);
#76=CONTEXT_DEPENDENT_SHAPE_REPRESENTATION(#52,#13253);
#77=CONTEXT_DEPENDENT_SHAPE_REPRESENTATION(#53,#13254);
#78=CONTEXT_DEPENDENT_SHAPE_REPRESENTATION(#54,#13255);
#79=CONTEXT_DEPENDENT_SHAPE_REPRESENTATION(#55,#13256);
#80=CONTEXT_DEPENDENT_SHAPE_REPRESENTATION(#56,#13257);
#81=CONTEXT_DEPENDENT_SHAPE_REPRESENTATION(#57,#13258);
#82=CONTEXT_DEPENDENT_SHAPE_REPRESENTATION(#58,#13259);
#83=CONTEXT_DEPENDENT_SHAPE_REPRESENTATION(#59,#13268);
#84=CONTEXT_DEPENDENT_SHAPE_REPRESENTATION(#60,#13269);
#85=CONTEXT_DEPENDENT_SHAPE_REPRESENTATION(#61,#13270);
#86=CONTEXT_DEPENDENT_SHAPE_REPRESENTATION(#62,#13271);
#87=CONTEXT_DEPENDENT_SHAPE_REPRESENTATION(#63,#13272);
#88=CONTEXT_DEPENDENT_SHAPE_REPRESENTATION(#64,#13273);
#89=CONTEXT_DEPENDENT_SHAPE_REPRESENTATION(#65,#13274);
#90=CONTEXT_DEPENDENT_SHAPE_REPRESENTATION(#66,#13275);
#91=CONTEXT_DEPENDENT_SHAPE_REPRESENTATION(#67,#13276);
#92=CONTEXT_DEPENDENT_SHAPE_REPRESENTATION(#68,#13277);
#93=NEXT_ASSEMBLY_USAGE_OCCURRENCE('Actuator 2 Cylinder:1',
'Actuator 2 Cylinder:1','Actuator 2 Cylinder:1',#13310,#13311,
'Actuator 2 Cylinder:1');
#94=NEXT_ASSEMBLY_USAGE_OCCURRENCE('Actuator 2 Piston Rod:1',
'Actuator 2 Piston Rod:1','Actuator 2 Piston Rod:1',#13310,#13312,
'Actuator 2 Piston Rod:1');
#95=NEXT_ASSEMBLY_USAGE_OCCURRENCE('Actuator 3 Cylinder:1',
'Actuator 3 Cylinder:1','Actuator 3 Cylinder:1',#13313,#13314,
'Actuator 3 Cylinder:1');
#96=NEXT_ASSEMBLY_USAGE_OCCURRENCE('Actuator 3 Piston Rod:1',
'Actuator 3 Piston Rod:1','Actuator 3 Piston Rod:1',#13313,#13315,
'Actuator 3 Piston Rod:1');
#97=NEXT_ASSEMBLY_USAGE_OCCURRENCE('Actuator 1 Cylinder:1',
'Actuator 1 Cylinder:1','Actuator 1 Cylinder:1',#13316,#13317,
'Actuator 1 Cylinder:1');
#98=NEXT_ASSEMBLY_USAGE_OCCURRENCE('Actuator 1 Piston Rod:1',
'Actuator 1 Piston Rod:1','Actuator 1 Piston Rod:1',#13316,#13318,
'Actuator 1 Piston Rod:1');
#99=NEXT_ASSEMBLY_USAGE_OCCURRENCE('Actuator 1 Holder:1',
'Actuator 1 Holder:1','Actuator 1 Holder:1',#13316,#13319,
'Actuator 1 Holder:1');
#100=NEXT_ASSEMBLY_USAGE_OCCURRENCE('Finger Link 1:1','Finger Link 1:1',
'Finger Link 1:1',#13306,#13307,'Finger Link 1:1');
#101=NEXT_ASSEMBLY_USAGE_OCCURRENCE('Finger Link 2:1','Finger Link 2:1',
'Finger Link 2:1',#13306,#13308,'Finger Link 2:1');
#102=NEXT_ASSEMBLY_USAGE_OCCURRENCE('Finger Link 3:1','Finger Link 3:1',
'Finger Link 3:1',#13306,#13309,'Finger Link 3:1');
#103=NEXT_ASSEMBLY_USAGE_OCCURRENCE('Pneumatic Actuator 2:1',
'Pneumatic Actuator 2:1','Pneumatic Actuator 2:1',#13306,#13310,
'Pneumatic Actuator 2:1');
#104=NEXT_ASSEMBLY_USAGE_OCCURRENCE('Pneumatic Actuator 3:1',
'Pneumatic Actuator 3:1','Pneumatic Actuator 3:1',#13306,#13313,
'Pneumatic Actuator 3:1');
#105=NEXT_ASSEMBLY_USAGE_OCCURRENCE('Pneumatic Actuator 1:1',
'Pneumatic Actuator 1:1','Pneumatic Actuator 1:1',#13306,#13316,
'Pneumatic Actuator 1:1');
#106=NEXT_ASSEMBLY_USAGE_OCCURRENCE('Finger Tip:1','Finger Tip:1',
'Finger Tip:1',#13306,#13320,'Finger Tip:1');
#107=NEXT_ASSEMBLY_USAGE_OCCURRENCE('Actuator 4 Cylinder:1',
'Actuator 4 Cylinder:1','Actuator 4 Cylinder:1',#13326,#13327,
'Actuator 4 Cylinder:1');
#108=NEXT_ASSEMBLY_USAGE_OCCURRENCE('Actuator 4 Piston Rod:1',
'Actuator 4 Piston Rod:1','Actuator 4 Piston Rod:1',#13326,#13328,
'Actuator 4 Piston Rod:1');
#109=NEXT_ASSEMBLY_USAGE_OCCURRENCE('Thumb Joint:1','Thumb Joint:1',
'Thumb Joint:1',#13321,#13322,'Thumb Joint:1');
#110=NEXT_ASSEMBLY_USAGE_OCCURRENCE('Thumb Link 1:1','Thumb Link 1:1',
'Thumb Link 1:1',#13321,#13323,'Thumb Link 1:1');
#111=NEXT_ASSEMBLY_USAGE_OCCURRENCE('Thumb Link 2:1','Thumb Link 2:1',
'Thumb Link 2:1',#13321,#13324,'Thumb Link 2:1');
#112=NEXT_ASSEMBLY_USAGE_OCCURRENCE('Thumb Tip:1','Thumb Tip:1',
'Thumb Tip:1',#13321,#13325,'Thumb Tip:1');
#113=NEXT_ASSEMBLY_USAGE_OCCURRENCE('Pneumatic Actuator 4:1',
'Pneumatic Actuator 4:1','Pneumatic Actuator 4:1',#13321,#13326,
'Pneumatic Actuator 4:1');
#114=NEXT_ASSEMBLY_USAGE_OCCURRENCE('Base:1','Base:1','Base:1',#13304,#13305,
'Base:1');
#115=NEXT_ASSEMBLY_USAGE_OCCURRENCE('Index Finger:1','Index Finger:1',
'Index Finger:1',#13304,#13306,'Index Finger:1');
#116=NEXT_ASSEMBLY_USAGE_OCCURRENCE('Thumb:1','Thumb:1','Thumb:1',#13304,
#13321,'Thumb:1');
#117=CONICAL_SURFACE('',#7216,13.,0.0174532925199433);
#118=CONICAL_SURFACE('',#7226,13.,0.0174532925199433);
#119=CONICAL_SURFACE('',#7291,11.7,0.0174532925199433);
#120=CONICAL_SURFACE('',#7299,11.7,0.0174532925199433);
#121=CONICAL_SURFACE('',#7376,10.4,0.0174532925199433);
#122=CONICAL_SURFACE('',#7390,10.4,0.0174532925199433);
#123=CONICAL_SURFACE('',#7682,14.3,0.0174532925199433);
#124=CONICAL_SURFACE('',#7720,14.3,0.0174532925199433);
#125=CONICAL_SURFACE('',#7729,14.3,0.0174532925199433);
#126=CONICAL_SURFACE('',#7753,14.3,0.0174532925199433);
#127=B_SPLINE_CURVE_WITH_KNOTS('',3,(#10160,#10161,#10162,#10163,#10164,
#10165,#10166,#10167,#10168,#10169,#10170,#10171,#10172,#10173,#10174,#10175,
#10176,#10177),.UNSPECIFIED.,.F.,.F.,(4,2,2,2,2,2,2,2,4),(-0.625948273254299,
-0.595286193065165,-0.532168206431192,-0.441842646589546,-0.3515170867479,
-0.261191526906255,-0.170865967064609,-0.107747980430636,-0.0770859002412175),
 .UNSPECIFIED.);
#128=B_SPLINE_CURVE_WITH_KNOTS('',3,(#10225,#10226,#10227,#10228,#10229,
#10230,#10231,#10232,#10233,#10234,#10235,#10236,#10237,#10238,#10239,#10240,
#10241,#10242),.UNSPECIFIED.,.F.,.F.,(4,2,2,2,2,2,2,2,4),(1.130849455016,
1.18732607982086,1.24380270462571,1.30024878607951,1.35669486753331,1.41336679321831,
1.4700387189033,1.52669509758432,1.58335147626535),.UNSPECIFIED.);
#129=B_SPLINE_CURVE_WITH_KNOTS('',3,(#10243,#10244,#10245,#10246,#10247,
#10248,#10249,#10250,#10251,#10252,#10253,#10254,#10255,#10256,#10257,#10258,
#10259,#10260,#10261),.UNSPECIFIED.,.F.,.F.,(4,2,2,2,3,2,2,2,4),(0.678347433766657,
0.735003812447681,0.791660191128705,0.848332116813698,0.905004042498691,
0.961450123952495,1.0178962054063,1.07437283021115,1.130849455016),
 .UNSPECIFIED.);
#130=B_SPLINE_CURVE_WITH_KNOTS('',3,(#10265,#10266,#10267,#10268,#10269,
#10270,#10271,#10272,#10273,#10274,#10275,#10276,#10277,#10278,#10279,#10280,
#10281,#10282),.UNSPECIFIED.,.F.,.F.,(4,2,2,2,2,2,2,2,4),(-0.678347433766657,
-0.621691055085633,-0.565034676404609,-0.508362750719616,-0.451690825034623,
-0.39524474358082,-0.338798662127016,-0.282322037322164,-0.225845412517312),
 .UNSPECIFIED.);
#131=B_SPLINE_CURVE_WITH_KNOTS('',3,(#10286,#10287,#10288,#10289,#10290,
#10291,#10292,#10293,#10294,#10295,#10296,#10297,#10298,#10299,#10300,#10301,
#10302,#10303,#10304),.UNSPECIFIED.,.F.,.F.,(4,2,2,2,3,2,2,2,4),(-0.225845412517312,
-0.169368787712459,-0.112892162907607,-0.0564460814538034,0.,0.0566719256849931,
0.113343851369986,0.17000023005101,0.226656608732034),.UNSPECIFIED.);
#132=B_SPLINE_CURVE_WITH_KNOTS('',3,(#10310,#10311,#10312,#10313),
 .UNSPECIFIED.,.F.,.F.,(4,4),(0.0270217399274549,0.0365389400069035),
 .UNSPECIFIED.);
#133=B_SPLINE_CURVE_WITH_KNOTS('',3,(#10315,#10316,#10317,#10318,#10319,
#10320,#10321,#10322,#10323,#10324,#10325,#10326,#10327,#10328,#10329,#10330,
#10331,#10332),.UNSPECIFIED.,.F.,.F.,(4,2,2,2,2,2,2,2,4),(4.40493642535816,
4.46219553041876,4.95875793037621,5.46800962865692,5.97726132693763,6.22066748237464,
6.46407363781164,6.95088594868566,7.16462957817159),.UNSPECIFIED.);
#134=B_SPLINE_CURVE_WITH_KNOTS('',3,(#10334,#10335,#10336,#10337,#10338,
#10339,#10340),.UNSPECIFIED.,.F.,.F.,(4,3,4),(0.0223867113798144,0.0254340142714909,
0.0283877461116507),.UNSPECIFIED.);
#135=B_SPLINE_CURVE_WITH_KNOTS('',3,(#10346,#10347,#10348,#10349,#10350,
#10351,#10352,#10353,#10354,#10355,#10356,#10357,#10358,#10359,#10360,#10361,
#10362,#10363,#10364,#10365,#10366,#10367,#10368,#10369,#10370,#10371),
 .UNSPECIFIED.,.F.,.F.,(4,2,2,2,2,2,2,2,2,2,2,2,4),(3.80610647446318,4.04439914990187,
4.28269182534056,4.75927717621793,5.2342149273987,5.47168380298909,5.70915267857947,
5.94662421983221,6.18409576108494,6.65903884359041,7.13562589625839,7.37391942259238,
7.61221294892637),.UNSPECIFIED.);
#136=B_SPLINE_CURVE_WITH_KNOTS('',3,(#10372,#10373,#10374,#10375,#10376,
#10377,#10378,#10379,#10380,#10381,#10382,#10383,#10384,#10385,#10386,#10387,
#10388,#10389,#10390,#10391,#10392,#10393,#10394,#10395,#10396,#10397),
 .UNSPECIFIED.,.F.,.F.,(4,2,2,2,2,2,2,2,2,2,2,2,4),(0.,0.238293526333989,
0.476587052667979,0.953174105335958,1.42811718784143,1.66558872909416,1.90306027034689,
2.14052914593728,2.37799802152767,2.85293577270844,3.32952112358581,3.5678137990245,
3.80610647446318),.UNSPECIFIED.);
#137=B_SPLINE_CURVE_WITH_KNOTS('',3,(#10401,#10402,#10403,#10404,#10405,
#10406,#10407),.UNSPECIFIED.,.F.,.F.,(4,3,4),(0.0224802824352469,0.0254340142749992,
0.0284813171662554),.UNSPECIFIED.);
#138=B_SPLINE_CURVE_WITH_KNOTS('',3,(#10409,#10410,#10411,#10412,#10413,
#10414,#10415,#10416,#10417,#10418,#10419,#10420,#10421,#10422,#10423,#10424,
#10425,#10426),.UNSPECIFIED.,.F.,.F.,(4,2,2,2,2,2,2,2,4),(0.766636682751041,
0.98038031223697,1.46719262311099,1.710598778548,1.95400493398501,2.46325663226571,
2.97250833054642,3.46907073050387,3.52632983556447),.UNSPECIFIED.);
#139=B_SPLINE_CURVE_WITH_KNOTS('',3,(#10427,#10428,#10429,#10430),
 .UNSPECIFIED.,.F.,.F.,(4,4),(0.0143722070064857,0.0238894070520057),
 .UNSPECIFIED.);
#140=B_SPLINE_CURVE_WITH_KNOTS('',3,(#10456,#10457,#10458,#10459,#10460,
#10461,#10462,#10463,#10464,#10465),.UNSPECIFIED.,.F.,.F.,(4,2,2,2,4),(3.52632983556447,
3.71735193048259,3.96563313046132,4.21391433044004,4.40493642535816),
 .UNSPECIFIED.);
#141=B_SPLINE_CURVE_WITH_KNOTS('',3,(#10617,#10618,#10619,#10620,#10621,
#10622,#10623,#10624,#10625,#10626,#10627,#10628,#10629,#10630,#10631,#10632,
#10633,#10634),.UNSPECIFIED.,.F.,.F.,(4,2,2,2,2,2,2,2,4),(1.0177645095144,
1.06859347183877,1.11942243416314,1.17022390747156,1.22102538077998,1.27203011389648,
1.32303484701297,1.37402558782589,1.42501632863882),.UNSPECIFIED.);
#142=B_SPLINE_CURVE_WITH_KNOTS('',3,(#10635,#10636,#10637,#10638,#10639,
#10640,#10641,#10642,#10643,#10644,#10645,#10646,#10647,#10648,#10649,#10650,
#10651,#10652,#10653),.UNSPECIFIED.,.F.,.F.,(4,2,2,2,3,2,2,2,4),(0.610512690389992,
0.661503431202914,0.712494172015835,0.763498905132329,0.814503638248823,
0.865305111557246,0.916106584865669,0.966935547190036,1.0177645095144),
 .UNSPECIFIED.);
#143=B_SPLINE_CURVE_WITH_KNOTS('',3,(#10657,#10658,#10659,#10660,#10661,
#10662,#10663,#10664,#10665,#10666,#10667,#10668,#10669,#10670,#10671,#10672,
#10673,#10674),.UNSPECIFIED.,.F.,.F.,(4,2,2,2,2,2,2,2,4),(-0.610512690389992,
-0.55952194957707,-0.508531208764149,-0.457526475647655,-0.406521742531161,
-0.355720269222738,-0.304918795914315,-0.254089833589948,-0.203260871265581),
 .UNSPECIFIED.);
#144=B_SPLINE_CURVE_WITH_KNOTS('',3,(#10678,#10679,#10680,#10681,#10682,
#10683,#10684,#10685,#10686,#10687,#10688,#10689,#10690,#10691,#10692,#10693,
#10694,#10695,#10696),.UNSPECIFIED.,.F.,.F.,(4,2,2,2,3,2,2,2,4),(-0.203260871265581,
-0.152431908941213,-0.101602946616846,-0.0508014733084231,0.,0.0510047331164938,
0.102009466232988,0.153000207045909,0.203990947858831),.UNSPECIFIED.);
#145=B_SPLINE_CURVE_WITH_KNOTS('',3,(#10702,#10703,#10704,#10705),
 .UNSPECIFIED.,.F.,.F.,(4,4),(0.0320334028505474,0.0349204253098787),
 .UNSPECIFIED.);
#146=B_SPLINE_CURVE_WITH_KNOTS('',3,(#10707,#10708,#10709,#10710,#10711,
#10712,#10713,#10714,#10715,#10716),.UNSPECIFIED.,.F.,.F.,(4,2,2,2,4),(1.8422488924149,
2.04440794331246,2.28720862023162,2.53000929715077,2.64124356821964),
 .UNSPECIFIED.);
#147=B_SPLINE_CURVE_WITH_KNOTS('',3,(#10718,#10719,#10720,#10721,#10722,
#10723,#10724,#10725,#10726,#10727),.UNSPECIFIED.,.F.,.F.,(4,2,2,2,4),(6.38658386410106,
6.48595628344589,6.66853921041904,6.85112213739218,7.0623660754825),
 .UNSPECIFIED.);
#148=B_SPLINE_CURVE_WITH_KNOTS('',3,(#10729,#10730,#10731,#10732,#10733,
#10734,#10735,#10736,#10737,#10738),.UNSPECIFIED.,.F.,.F.,(4,2,2,2,4),(3.96444278282234,
4.01597597737689,4.46288213733859,4.92120866579123,5.18441802586752),
 .UNSPECIFIED.);
#149=B_SPLINE_CURVE_WITH_KNOTS('',3,(#10740,#10741,#10742,#10743,#10744,
#10745,#10746),.UNSPECIFIED.,.F.,.F.,(4,3,4),(0.0201480402418329,0.0228906128443418,
0.0255489715004856),.UNSPECIFIED.);
#150=B_SPLINE_CURVE_WITH_KNOTS('',3,(#10752,#10753,#10754,#10755,#10756,
#10757,#10758,#10759,#10760,#10761,#10762,#10763,#10764,#10765,#10766,#10767,
#10768,#10769,#10770,#10771,#10772,#10773),.UNSPECIFIED.,.F.,.F.,(4,2,2,
2,2,2,2,2,2,2,4),(3.42549582701687,3.63995923491168,3.8544226428065,4.28334945859613,
4.71079343465883,5.13823741072153,5.56568618497645,5.99313495923137,6.42206330663255,
6.63652748033314,6.85099165403373),.UNSPECIFIED.);
#151=B_SPLINE_CURVE_WITH_KNOTS('',3,(#10774,#10775,#10776,#10777,#10778,
#10779,#10780,#10781,#10782,#10783,#10784,#10785,#10786,#10787,#10788,#10789,
#10790,#10791,#10792,#10793,#10794,#10795),.UNSPECIFIED.,.F.,.F.,(4,2,2,
2,2,2,2,2,2,2,4),(0.,0.21446417370059,0.428928347401181,0.857856694802362,
1.28530546905728,1.7127542433122,2.1401982193749,2.5676421954376,2.99656901122723,
3.21103241912205,3.42549582701687),.UNSPECIFIED.);
#152=B_SPLINE_CURVE_WITH_KNOTS('',3,(#10799,#10800,#10801,#10802,#10803,
#10804,#10805),.UNSPECIFIED.,.F.,.F.,(4,3,4),(0.0202322541917222,0.0228906128474993,
0.0256331854496299),.UNSPECIFIED.);
#153=B_SPLINE_CURVE_WITH_KNOTS('',3,(#10807,#10808,#10809,#10810,#10811,
#10812,#10813,#10814,#10815,#10816),.UNSPECIFIED.,.F.,.F.,(4,2,2,2,4),(1.95372160896285,
2.21693096903914,2.67525749749178,3.12216365745348,3.17369685200803),
 .UNSPECIFIED.);
#154=B_SPLINE_CURVE_WITH_KNOTS('',3,(#10818,#10819,#10820,#10821,#10822,
#10823,#10824,#10825,#10826,#10827),.UNSPECIFIED.,.F.,.F.,(4,2,2,2,4),(10.2613045765272,
10.4725485146175,10.6551314415907,10.8377143685638,10.9370867879086),
 .UNSPECIFIED.);
#155=B_SPLINE_CURVE_WITH_KNOTS('',3,(#10829,#10830,#10831,#10832,#10833,
#10834,#10835,#10836,#10837,#10838),.UNSPECIFIED.,.F.,.F.,(4,2,2,2,4),(4.03342707380782,
4.14466134487669,4.38746202179585,4.630262698715,4.83242174961257),
 .UNSPECIFIED.);
#156=B_SPLINE_CURVE_WITH_KNOTS('',3,(#10839,#10840,#10841,#10842),
 .UNSPECIFIED.,.F.,.F.,(4,4),(0.0108996070094278,0.0137866294584668),
 .UNSPECIFIED.);
#157=B_SPLINE_CURVE_WITH_KNOTS('',3,(#10848,#10849,#10850,#10851,#10852,
#10853,#10854,#10855,#10856,#10857),.UNSPECIFIED.,.F.,.F.,(4,2,2,2,4),(-3.96444278282234,
-3.79252289739604,-3.56906981741519,-3.34561673743433,-3.17369685200803),
 .UNSPECIFIED.);
#158=B_SPLINE_CURVE_WITH_KNOTS('',3,(#10897,#10898,#10899,#10900,#10901,
#10902,#10903,#10904,#10905,#10906,#10907,#10908,#10909),.UNSPECIFIED.,
 .F.,.F.,(4,2,2,2,3,4),(-0.346533453564935,-0.234184438198016,-0.144253134532049,
-0.0681159640541859,0.,0.00346167201765239),.UNSPECIFIED.);
#159=B_SPLINE_CURVE_WITH_KNOTS('',3,(#10914,#10915,#10916,#10917,#10918,
#10919,#10920,#10921,#10922,#10923,#10924,#10925,#10926),.UNSPECIFIED.,
 .F.,.F.,(4,3,2,2,2,4),(-0.003464253118063,0.,0.0681159640541862,0.14425313453205,
0.234184438198017,0.346533453564935),.UNSPECIFIED.);
#160=B_SPLINE_CURVE_WITH_KNOTS('',3,(#11078,#11079,#11080,#11081,#11082,
#11083,#11084,#11085,#11086,#11087,#11088,#11089,#11090,#11091,#11092,#11093,
#11094,#11095),.UNSPECIFIED.,.F.,.F.,(4,2,2,2,2,2,2,2,4),(0.904679564012803,
0.949860863856685,0.995042163700566,1.04019902886361,1.08535589402665,1.13069343457465,
1.17603097512264,1.22135607806746,1.26668118101228),.UNSPECIFIED.);
#161=B_SPLINE_CURVE_WITH_KNOTS('',3,(#11096,#11097,#11098,#11099,#11100,
#11101,#11102,#11103,#11104,#11105,#11106,#11107,#11108,#11109,#11110,#11111,
#11112,#11113,#11114),.UNSPECIFIED.,.F.,.F.,(4,2,2,2,3,2,2,2,4),(0.542677947013326,
0.588003049958145,0.633328152902964,0.678665693450959,0.724003233998953,
0.769160099161996,0.814316964325039,0.859498264168921,0.904679564012803),
 .UNSPECIFIED.);
#162=B_SPLINE_CURVE_WITH_KNOTS('',3,(#11118,#11119,#11120,#11121,#11122,
#11123,#11124,#11125,#11126,#11127,#11128,#11129,#11130,#11131,#11132,#11133,
#11134,#11135),.UNSPECIFIED.,.F.,.F.,(4,2,2,2,2,2,2,2,4),(-0.542677947013326,
-0.497352844068507,-0.452027741123688,-0.406690200575693,-0.361352660027699,
-0.316195794864656,-0.271038929701613,-0.225857629857731,-0.180676330013849),
 .UNSPECIFIED.);
#163=B_SPLINE_CURVE_WITH_KNOTS('',3,(#11139,#11140,#11141,#11142,#11143,
#11144,#11145,#11146,#11147,#11148,#11149,#11150,#11151,#11152,#11153,#11154,
#11155,#11156,#11157),.UNSPECIFIED.,.F.,.F.,(4,2,2,2,3,2,2,2,4),(-0.180676330013849,
-0.135495030169968,-0.0903137303260857,-0.0451568651630429,0.,0.0453375405479944,
0.0906750810959889,0.136000184040808,0.181325286985627),.UNSPECIFIED.);
#164=B_SPLINE_CURVE_WITH_KNOTS('',3,(#11163,#11164,#11165,#11166),
 .UNSPECIFIED.,.F.,.F.,(4,4),(0.0291654849228324,0.031266531407063),
 .UNSPECIFIED.);
#165=B_SPLINE_CURVE_WITH_KNOTS('',3,(#11168,#11169,#11170,#11171,#11172,
#11173,#11174,#11175),.UNSPECIFIED.,.F.,.F.,(4,2,2,4),(0.276435365996458,
0.375879882596353,0.487798645153617,0.537259984529731),.UNSPECIFIED.);
#166=B_SPLINE_CURVE_WITH_KNOTS('',3,(#11177,#11178,#11179,#11180),
 .UNSPECIFIED.,.F.,.F.,(4,4),(1.06524753198133,1.38156085898599),
 .UNSPECIFIED.);
#167=B_SPLINE_CURVE_WITH_KNOTS('',3,(#11182,#11183,#11184,#11185,#11186,
#11187),.UNSPECIFIED.,.F.,.F.,(4,2,4),(1.75246957687291,1.78785142251735,
1.90812306822259),.UNSPECIFIED.);
#168=B_SPLINE_CURVE_WITH_KNOTS('',3,(#11189,#11190,#11191,#11192,#11193,
#11194,#11195,#11196,#11197,#11198),.UNSPECIFIED.,.F.,.F.,(4,2,2,2,4),(5.98774864501298,
5.99007118193337,6.16584174870578,6.34161231547819,6.60463416407235),
 .UNSPECIFIED.);
#169=B_SPLINE_CURVE_WITH_KNOTS('',3,(#11200,#11201,#11202,#11203,#11204,
#11205,#11206,#11207,#11208,#11209),.UNSPECIFIED.,.F.,.F.,(4,2,2,2,4),(3.5239413534678,
3.56975642433501,3.96700634430097,4.37440770292553,4.58682119202782),
 .UNSPECIFIED.);
#170=B_SPLINE_CURVE_WITH_KNOTS('',3,(#11211,#11212,#11213,#11214,#11215,
#11216,#11217),.UNSPECIFIED.,.F.,.F.,(4,3,4),(0.0179093691038515,0.0203472114171927,
0.0227101968893206),.UNSPECIFIED.);
#171=B_SPLINE_CURVE_WITH_KNOTS('',3,(#11223,#11224,#11225,#11226,#11227,
#11228,#11229,#11230,#11231,#11232,#11233,#11234,#11235,#11236,#11237,#11238,
#11239,#11240),.UNSPECIFIED.,.F.,.F.,(4,2,2,2,2,2,2,2,4),(3.04488517957055,
3.42615346027245,3.80742174097434,4.18737194191896,4.56732214286358,4.94727660886795,
5.32723107487233,5.70850071700671,6.08977035914109),.UNSPECIFIED.);
#172=B_SPLINE_CURVE_WITH_KNOTS('',3,(#11241,#11242,#11243,#11244,#11245,
#11246,#11247,#11248,#11249,#11250,#11251,#11252,#11253,#11254,#11255,#11256,
#11257,#11258),.UNSPECIFIED.,.F.,.F.,(4,2,2,2,2,2,2,2,4),(0.,0.381269642134383,
0.762539284268766,1.14249375027314,1.52244821627752,1.90239841722213,2.28234861816675,
2.66361689886865,3.04488517957055),.UNSPECIFIED.);
#173=B_SPLINE_CURVE_WITH_KNOTS('',3,(#11262,#11263,#11264,#11265,#11266,
#11267,#11268),.UNSPECIFIED.,.F.,.F.,(4,3,4),(0.0179842259481975,0.0203472114199994,
0.0227850537330044),.UNSPECIFIED.);
#174=B_SPLINE_CURVE_WITH_KNOTS('',3,(#11270,#11271,#11272,#11273,#11274,
#11275,#11276,#11277,#11278,#11279),.UNSPECIFIED.,.F.,.F.,(4,2,2,2,4),(1.75819181671029,
1.97060530581257,2.37800666443714,2.7752565844031,2.82107165527031),
 .UNSPECIFIED.);
#175=B_SPLINE_CURVE_WITH_KNOTS('',3,(#11281,#11282,#11283,#11284,#11285,
#11286,#11287,#11288,#11289,#11290),.UNSPECIFIED.,.F.,.F.,(4,2,2,2,4),(9.36812303237173,
9.63114488096588,9.80691544773829,9.9826860145107,9.98500855143109),
 .UNSPECIFIED.);
#176=B_SPLINE_CURVE_WITH_KNOTS('',3,(#11292,#11293,#11294,#11295,#11296,
#11297),.UNSPECIFIED.,.F.,.F.,(4,2,4),(4.24121592260514,4.36148756831038,
4.39686941395482),.UNSPECIFIED.);
#177=B_SPLINE_CURVE_WITH_KNOTS('',3,(#11299,#11300,#11301,#11302),
 .UNSPECIFIED.,.F.,.F.,(4,4),(5.68043931343762,5.99675264044228),
 .UNSPECIFIED.);
#178=B_SPLINE_CURVE_WITH_KNOTS('',3,(#11304,#11305,#11306,#11307,#11308,
#11309,#11310,#11311),.UNSPECIFIED.,.F.,.F.,(4,2,2,4),(1.76236608590955,
1.81182742528566,1.92374618784292,2.02319070444282),.UNSPECIFIED.);
#179=B_SPLINE_CURVE_WITH_KNOTS('',3,(#11312,#11313,#11314,#11315),
 .UNSPECIFIED.,.F.,.F.,(4,4),(0.0094623862109046,0.0115634326876449),
 .UNSPECIFIED.);
#180=B_SPLINE_CURVE_WITH_KNOTS('',3,(#11332,#11333,#11334,#11335,#11336,
#11337,#11338,#11339,#11340,#11341,#11342,#11343,#11344),.UNSPECIFIED.,
 .F.,.F.,(4,3,2,2,2,4),(1.6015262701395,1.6049878447796,1.6729249721852,
1.74884321655348,1.83898176381711,1.95424158697802),.UNSPECIFIED.);
#181=B_SPLINE_CURVE_WITH_KNOTS('',3,(#11345,#11346,#11347,#11348,#11349,
#11350,#11351,#11352,#11353,#11354,#11355,#11356,#11357),.UNSPECIFIED.,
 .F.,.F.,(4,2,2,2,3,4),(1.25494218036839,1.36265497339682,1.4481494572272,
1.53110216280993,1.60422001043371,1.60768158507379),.UNSPECIFIED.);
#182=B_SPLINE_CURVE_WITH_KNOTS('',3,(#11359,#11360,#11361,#11362,#11363,
#11364,#11365,#11366,#11367,#11368,#11369,#11370,#11371,#11372,#11373,#11374,
#11375,#11376,#11377,#11378,#11379,#11380,#11381,#11382,#11383,#11384,#11385,
#11386,#11387,#11388,#11389,#11390,#11391,#11392,#11393,#11394,#11395,#11396,
#11397,#11398,#11399,#11400,#11401,#11402,#11403,#11404,#11405,#11406,#11407,
#11408,#11409,#11410),.UNSPECIFIED.,.T.,.F.,(4,2,2,2,2,2,2,2,2,2,2,2,2,
2,2,2,2,2,2,2,2,2,2,2,2,4),(-0.41069396663975,-0.366983311744642,-0.333124597039194,
-0.316725158605419,-0.311400724276707,-0.308795794387217,-0.307003152587989,
-0.305253095176476,-0.302970204179655,-0.299167956861605,-0.28993505003161,
-0.264304988598304,-0.228809697804181,-0.190091960609317,-0.153364093718904,
-0.124905530199035,-0.112501594518716,-0.107965577825246,-0.105609428487505,
-0.103889729748576,-0.102119162499972,-0.0996651361174354,-0.0953267397354206,
-0.0781357693656503,-0.0445945135149615,0.),.UNSPECIFIED.);
#183=B_SPLINE_CURVE_WITH_KNOTS('',3,(#11416,#11417,#11418,#11419,#11420,
#11421),.UNSPECIFIED.,.F.,.F.,(4,2,4),(-3.5239413534678,-3.17250650436905,
-2.82107165527031),.UNSPECIFIED.);
#184=B_SPLINE_CURVE_WITH_KNOTS('',3,(#11947,#11948,#11949,#11950,#11951,
#11952,#11953,#11954,#11955,#11956,#11957,#11958,#11959,#11960,#11961,#11962,
#11963,#11964,#11965,#11966,#11967,#11968,#11969),.UNSPECIFIED.,.F.,.F.,
(4,2,2,2,2,3,2,2,2,2,4),(0.476645491037206,0.489023957516382,0.527166589495669,
0.568095012367448,0.607142264956957,0.636252225893218,0.674200453389387,
0.713373161852222,0.750226922703377,0.78797801482852,0.795881712617993),
 .UNSPECIFIED.);
#185=B_SPLINE_CURVE_WITH_KNOTS('',3,(#11970,#11971,#11972,#11973,#11974,
#11975,#11976,#11977,#11978,#11979,#11980,#11981,#11982,#11983,#11984,#11985,
#11986,#11987,#11988,#11989),.UNSPECIFIED.,.F.,.F.,(4,2,2,2,2,2,2,2,2,4),
(0.159629486724776,0.18739470215505,0.223766252646954,0.263805807870951,
0.302029537123351,0.34097527431584,0.380812071035441,0.417115871073174,
0.453232846571769,0.476645491037206),.UNSPECIFIED.);
#186=B_SPLINE_CURVE_WITH_KNOTS('',3,(#11993,#11994,#11995,#11996,#11997,
#11998,#11999,#12000,#12001,#12002,#12003,#12004,#12005,#12006,#12007,#12008,
#12009,#12010,#12011,#12012,#12013,#12014,#12015),.UNSPECIFIED.,.F.,.F.,
(4,2,2,2,2,3,2,2,2,2,4),(0.476645491037025,0.48902395751638,0.527166589495666,
0.568095012367448,0.607142264956952,0.636252225893214,0.674200453389384,
0.713373161852219,0.75022692270337,0.78797801482851,0.795881712618303),
 .UNSPECIFIED.);
#187=B_SPLINE_CURVE_WITH_KNOTS('',3,(#12019,#12020,#12021,#12022,#12023,
#12024,#12025,#12026,#12027,#12028,#12029,#12030,#12031,#12032,#12033,#12034,
#12035,#12036,#12037,#12038),.UNSPECIFIED.,.F.,.F.,(4,2,2,2,2,2,2,2,2,4),
(0.795881712618303,0.823646928048259,0.860018478540157,0.900058033764149,
0.938281763016554,0.977227500209047,1.01706429692865,1.05336809696638,1.08948507246498,
1.11289771693024),.UNSPECIFIED.);
#188=B_SPLINE_CURVE_WITH_KNOTS('',3,(#12098,#12099,#12100,#12101,#12102,
#12103,#12104,#12105,#12106,#12107,#12108,#12109,#12110,#12111,#12112,#12113,
#12114,#12115,#12116,#12117,#12118,#12119,#12120,#12121,#12122,#12123,#12124,
#12125,#12126,#12127,#12128,#12129,#12130,#12131,#12132,#12133,#12134,#12135,
#12136,#12137,#12138),.UNSPECIFIED.,.T.,.F.,(4,2,2,2,2,2,3,2,2,2,2,2,2,
2,2,2,2,2,2,4),(4.76570010814283,4.82373748195937,5.15211023194195,5.51811468114358,
5.92483477190322,6.13853392596326,6.35204429850806,6.71291359634487,7.09425816350559,
7.50552237110612,7.8592853831874,8.18933065337909,8.53450621361463,8.93047115205954,
9.32063251608662,9.68763081499438,10.0531628494056,10.4503791856812,10.8359489090294,
11.1177444066509),.UNSPECIFIED.);
#189=B_SPLINE_CURVE_WITH_KNOTS('',3,(#12314,#12315,#12316,#12317,#12318,
#12319,#12320,#12321,#12322,#12323,#12324,#12325,#12326,#12327,#12328,#12329,
#12330,#12331),.UNSPECIFIED.,.F.,.F.,(4,2,2,2,2,2,2,2,4),(1.2439344005176,
1.30605868780294,1.36818297508828,1.43027366468746,1.49236435428665,1.55470347254014,
1.61704259079363,1.67936460734276,1.74168662389188),.UNSPECIFIED.);
#190=B_SPLINE_CURVE_WITH_KNOTS('',3,(#12332,#12333,#12334,#12335,#12336,
#12337,#12338,#12339,#12340,#12341,#12342,#12343,#12344,#12345,#12346,#12347,
#12348,#12349,#12350),.UNSPECIFIED.,.F.,.F.,(4,2,2,2,3,2,2,2,4),(0.746182177143323,
0.80850419369245,0.870826210241576,0.933165328495069,0.995504446748561,
1.05759513634774,1.11968582594693,1.18181011323227,1.2439344005176),
 .UNSPECIFIED.);
#191=B_SPLINE_CURVE_WITH_KNOTS('',3,(#12354,#12355,#12356,#12357,#12358,
#12359,#12360,#12361,#12362,#12363,#12364,#12365,#12366,#12367,#12368,#12369,
#12370,#12371),.UNSPECIFIED.,.F.,.F.,(4,2,2,2,2,2,2,2,4),(-0.746182177143323,
-0.683860160594197,-0.621538144045071,-0.559199025791578,-0.496859907538086,
-0.434769217938902,-0.372678528339718,-0.310554241054381,-0.248429953769043),
 .UNSPECIFIED.);
#192=B_SPLINE_CURVE_WITH_KNOTS('',3,(#12375,#12376,#12377,#12378,#12379,
#12380,#12381,#12382,#12383,#12384,#12385,#12386,#12387,#12388,#12389,#12390,
#12391,#12392,#12393),.UNSPECIFIED.,.F.,.F.,(4,2,2,2,3,2,2,2,4),(-0.248429953769043,
-0.186305666483705,-0.124181379198368,-0.0620906895991839,0.,0.0623391182534924,
0.124678236506985,0.187000253056111,0.249322269605238),.UNSPECIFIED.);
#193=B_SPLINE_CURVE_WITH_KNOTS('',3,(#12409,#12410,#12411,#12412,#12413,
#12414,#12415,#12416,#12417,#12418,#12419,#12420,#12421,#12422),
 .UNSPECIFIED.,.F.,.F.,(4,2,2,2,2,2,4),(6.66820605648738,6.76341848404012,
7.03258976532484,7.57093232789428,8.11497235847169,8.3869923737604,8.50692180294266),
 .UNSPECIFIED.);
#194=B_SPLINE_CURVE_WITH_KNOTS('',3,(#12426,#12427,#12428,#12429,#12430,
#12431,#12432,#12433,#12434,#12435,#12436,#12437,#12438,#12439),
 .UNSPECIFIED.,.F.,.F.,(4,2,2,2,2,2,4),(0.152090586106455,0.272020015288707,
0.544040030577415,1.08808006115483,1.62642262372427,1.89559390500899,1.99080633256173),
 .UNSPECIFIED.);
#195=B_SPLINE_CURVE_WITH_KNOTS('',3,(#12452,#12453,#12454,#12455,#12456,
#12457,#12458,#12459,#12460,#12461,#12462,#12463,#12464,#12465,#12466,#12467,
#12468,#12469,#12470,#12471,#12472,#12473,#12474,#12475,#12476,#12477),
 .UNSPECIFIED.,.F.,.F.,(4,2,2,2,2,2,2,2,2,2,2,2,4),(2.33883536058546,2.43393235013178,
2.70309951396985,3.24143384164599,3.78547001808527,4.05748810630491,4.32950619452455,
4.6015242827442,4.87354237096384,5.41757854740312,5.95591287507926,6.22508003891732,
6.32017702846365),.UNSPECIFIED.);
#196=B_SPLINE_CURVE_WITH_KNOTS('',3,(#12487,#12488,#12489,#12490,#12491,
#12492,#12493),.UNSPECIFIED.,.F.,.F.,(4,3,4),(0.0272601210138638,0.0280070000945348,
0.0403698029815644),.UNSPECIFIED.);
#197=B_SPLINE_CURVE_WITH_KNOTS('',3,(#12495,#12496,#12497,#12498,#12499,
#12500,#12501,#12502,#12503,#12504,#12505,#12506,#12507,#12508,#12509,#12510,
#12511,#12512,#12513,#12514,#12515,#12516,#12517,#12518,#12519,#12520,#12521,
#12522,#12523,#12524,#12525,#12526,#12527,#12528,#12529,#12530,#12531,#12532,
#12533,#12534,#12535,#12536),.UNSPECIFIED.,.F.,.F.,(4,2,2,2,2,2,2,2,2,2,
2,2,2,2,2,2,2,2,2,2,4),(0.895792364322182,1.15266269025927,1.7130326392156,
1.99321761369377,2.27340258817193,2.55312809524007,2.8328536023082,3.39230461644446,
3.9653006408784,4.25179865309537,4.53829666531233,4.8247946775293,5.11129268974627,
5.6842887141802,6.24373972831647,6.5234652353846,6.80319074245273,7.08415066001029,
7.36511057756785,7.92703041268297,8.1809357022053),.UNSPECIFIED.);
#198=B_SPLINE_CURVE_WITH_KNOTS('',3,(#12538,#12539,#12540,#12541,#12542,
#12543,#12544),.UNSPECIFIED.,.F.,.F.,(4,3,4),(0.01564419735118,0.0280070001942108,
0.0287538792722237),.UNSPECIFIED.);
#199=B_SPLINE_CURVE_WITH_KNOTS('',3,(#12595,#12596,#12597,#12598,#12599,
#12600,#12601,#12602,#12603,#12604,#12605,#12606,#12607,#12608,#12609,#12610,
#12611,#12612,#12613,#12614),.UNSPECIFIED.,.F.,.F.,(4,2,2,2,2,2,2,2,2,4),
(1.13069615346588,1.18716968917911,1.24364799854408,1.30009527290761,1.35654254727113,
1.41319810974912,1.46985367222711,1.526495709458,1.58313774668889,1.58314252031411),
 .UNSPECIFIED.);
#200=B_SPLINE_CURVE_WITH_KNOTS('',3,(#12615,#12616,#12617,#12618,#12619,
#12620,#12621,#12622,#12623,#12624,#12625,#12626,#12627,#12628,#12629,#12630,
#12631,#12632,#12633,#12634,#12635),.UNSPECIFIED.,.F.,.F.,(4,2,2,2,3,2,
2,2,2,4),(0.678287603396378,0.734918137493847,0.791553445216531,0.848204181067131,
0.904854916917731,0.961302354464157,1.01774979201058,1.07422058591236,1.13069137981413,
1.13069615346588),.UNSPECIFIED.);
#201=B_SPLINE_CURVE_WITH_KNOTS('',3,(#12639,#12640,#12641,#12642,#12643,
#12644,#12645,#12646,#12647,#12648,#12649,#12650,#12651,#12652,#12653,#12654,
#12655,#12656,#12657,#12658),.UNSPECIFIED.,.F.,.F.,(4,2,2,2,2,2,2,2,2,4),
(-0.678287603396414,-0.678282829771164,-0.621640792540269,-0.564998755309374,
-0.508343192831388,-0.451687630353401,-0.395240355989875,-0.338793081626349,
-0.282314772261376,-0.225841236548144),.UNSPECIFIED.);
#202=B_SPLINE_CURVE_WITH_KNOTS('',3,(#12662,#12663,#12664,#12665,#12666,
#12667,#12668,#12669,#12670,#12671,#12672,#12673,#12674,#12675,#12676,#12677,
#12678,#12679,#12680,#12681,#12682),.UNSPECIFIED.,.F.,.F.,(4,2,2,2,2,3,
2,2,2,4),(-0.225841236548144,-0.225836462896404,-0.169365668994628,-0.112894875092852,
-0.0564474375464262,0.,0.0566507358506003,0.113301471701201,0.169936779423884,
0.226567313521317),.UNSPECIFIED.);
#203=B_SPLINE_CURVE_WITH_KNOTS('',3,(#12686,#12687,#12688,#12689,#12690,
#12691,#12692,#12693,#12694,#12695,#12696,#12697,#12698,#12699,#12700,#12701,
#12702,#12703),.UNSPECIFIED.,.F.,.F.,(4,2,2,2,2,2,2,2,4),(-0.688543100579729,
-0.654814812371682,-0.585385027074312,-0.486026911248501,-0.386668795422691,
-0.287310679596881,-0.18795256377107,-0.1185227784737,-0.0847944902653396),
 .UNSPECIFIED.);
#204=B_SPLINE_CURVE_WITH_KNOTS('',3,(#12742,#12743,#12744,#12745,#12746,
#12747,#12748,#12749,#12750,#12751),.UNSPECIFIED.,.F.,.F.,(4,2,2,2,4),(2.79683412091131,
2.83278881190682,3.39223982604309,3.96523585047702,4.02795363969691),
 .UNSPECIFIED.);
#205=B_SPLINE_CURVE_WITH_KNOTS('',3,(#12753,#12754,#12755,#12756,#12757,
#12758,#12759,#12760,#12761,#12762),.UNSPECIFIED.,.F.,.F.,(4,2,2,2,4),(10.3179905566208,
10.457151700737,10.6290799698098,10.8010082388826,10.8999538958969),
 .UNSPECIFIED.);
#206=B_SPLINE_CURVE_WITH_KNOTS('',3,(#12764,#12765,#12766,#12767,#12768,
#12769,#12770,#12771,#12772,#12773,#12774,#12775,#12776,#12777),
 .UNSPECIFIED.,.F.,.F.,(4,2,2,2,2,2,4),(-7.02551957351303,-6.83439163802274,
-6.07684267508665,-5.67712314178527,-5.27740360848388,-4.91546143594968,
-4.72326894801671),.UNSPECIFIED.);
#207=B_SPLINE_CURVE_WITH_KNOTS('',3,(#12789,#12790,#12791,#12792,#12793,
#12794,#12795,#12796,#12797,#12798,#12799,#12800,#12801,#12802),
 .UNSPECIFIED.,.F.,.F.,(4,2,2,2,2,2,4),(-4.38376957881428,-4.1915770908813,
-3.82963491834711,-3.42991538504572,-3.03019585174433,-2.27264688880825,
-2.08151895331795),.UNSPECIFIED.);
#208=B_SPLINE_CURVE_WITH_KNOTS('',3,(#12804,#12805,#12806,#12807,#12808,
#12809,#12810,#12811,#12812,#12813),.UNSPECIFIED.,.F.,.F.,(4,2,2,2,4),(6.41116921174888,
6.5101148687632,6.68204313783601,6.85397140690883,6.993132551025),
 .UNSPECIFIED.);
#209=B_SPLINE_CURVE_WITH_KNOTS('',3,(#12815,#12816,#12817,#12818,#12819,
#12820,#12821,#12822,#12823,#12824),.UNSPECIFIED.,.F.,.F.,(4,2,2,2,4),(5.02250397090605,
5.11122789934489,5.68422392377882,6.24367493791509,6.2796296289106),
 .UNSPECIFIED.);
#210=B_SPLINE_CURVE_WITH_KNOTS('',3,(#12831,#12832,#12833,#12834,#12835),
 .UNSPECIFIED.,.F.,.F.,(4,1,4),(0.0247143916721011,0.0279654930527155,0.0312302909052024),
 .UNSPECIFIED.);
#211=B_SPLINE_CURVE_WITH_KNOTS('',3,(#12862,#12863,#12864,#12865,#12866,
#12867,#12868,#12869,#12870,#12871),.UNSPECIFIED.,.F.,.F.,(4,2,2,2,4),(4.05396350737764,
4.25173386269399,4.53823187491096,4.82472988712792,5.02250024244427),
 .UNSPECIFIED.);
#212=SHAPE_REPRESENTATION_RELATIONSHIP('SRR','None',#13279,#230);
#213=SHAPE_REPRESENTATION_RELATIONSHIP('SRR','None',#13281,#231);
#214=SHAPE_REPRESENTATION_RELATIONSHIP('SRR','None',#13282,#232);
#215=SHAPE_REPRESENTATION_RELATIONSHIP('SRR','None',#13283,#233);
#216=SHAPE_REPRESENTATION_RELATIONSHIP('SRR','None',#13285,#234);
#217=SHAPE_REPRESENTATION_RELATIONSHIP('SRR','None',#13286,#235);
#218=SHAPE_REPRESENTATION_RELATIONSHIP('SRR','None',#13288,#236);
#219=SHAPE_REPRESENTATION_RELATIONSHIP('SRR','None',#13289,#237);
#220=SHAPE_REPRESENTATION_RELATIONSHIP('SRR','None',#13291,#238);
#221=SHAPE_REPRESENTATION_RELATIONSHIP('SRR','None',#13292,#239);
#222=SHAPE_REPRESENTATION_RELATIONSHIP('SRR','None',#13293,#240);
#223=SHAPE_REPRESENTATION_RELATIONSHIP('SRR','None',#13294,#241);
#224=SHAPE_REPRESENTATION_RELATIONSHIP('SRR','None',#13296,#242);
#225=SHAPE_REPRESENTATION_RELATIONSHIP('SRR','None',#13297,#243);
#226=SHAPE_REPRESENTATION_RELATIONSHIP('SRR','None',#13298,#244);
#227=SHAPE_REPRESENTATION_RELATIONSHIP('SRR','None',#13299,#245);
#228=SHAPE_REPRESENTATION_RELATIONSHIP('SRR','None',#13301,#246);
#229=SHAPE_REPRESENTATION_RELATIONSHIP('SRR','None',#13302,#247);
#230=ADVANCED_BREP_SHAPE_REPRESENTATION('',(#266),#13175);
#231=ADVANCED_BREP_SHAPE_REPRESENTATION('',(#267),#13177);
#232=ADVANCED_BREP_SHAPE_REPRESENTATION('',(#268),#13178);
#233=ADVANCED_BREP_SHAPE_REPRESENTATION('',(#269),#13179);
#234=ADVANCED_BREP_SHAPE_REPRESENTATION('',(#270),#13181);
#235=ADVANCED_BREP_SHAPE_REPRESENTATION('',(#271),#13182);
#236=ADVANCED_BREP_SHAPE_REPRESENTATION('',(#272),#13184);
#237=ADVANCED_BREP_SHAPE_REPRESENTATION('',(#273),#13185);
#238=ADVANCED_BREP_SHAPE_REPRESENTATION('',(#274),#13187);
#239=ADVANCED_BREP_SHAPE_REPRESENTATION('',(#275),#13188);
#240=ADVANCED_BREP_SHAPE_REPRESENTATION('',(#276),#13189);
#241=ADVANCED_BREP_SHAPE_REPRESENTATION('',(#277),#13190);
#242=ADVANCED_BREP_SHAPE_REPRESENTATION('',(#278),#13192);
#243=ADVANCED_BREP_SHAPE_REPRESENTATION('',(#279),#13193);
#244=ADVANCED_BREP_SHAPE_REPRESENTATION('',(#280),#13194);
#245=ADVANCED_BREP_SHAPE_REPRESENTATION('',(#281),#13195);
#246=ADVANCED_BREP_SHAPE_REPRESENTATION('',(#282),#13197);
#247=ADVANCED_BREP_SHAPE_REPRESENTATION('',(#283),#13198);
#248=STYLED_ITEM('',(#13408),#266);
#249=STYLED_ITEM('',(#13409),#267);
#250=STYLED_ITEM('',(#13409),#268);
#251=STYLED_ITEM('',(#13409),#269);
#252=STYLED_ITEM('',(#13409),#270);
#253=STYLED_ITEM('',(#13409),#271);
#254=STYLED_ITEM('',(#13410),#272);
#255=STYLED_ITEM('',(#13411),#273);
#256=STYLED_ITEM('',(#13410),#274);
#257=STYLED_ITEM('',(#13410),#275);
#258=STYLED_ITEM('',(#13409),#276);
#259=STYLED_ITEM('',(#13409),#277);
#260=STYLED_ITEM('',(#13410),#278);
#261=STYLED_ITEM('',(#13411),#279);
#262=STYLED_ITEM('',(#13409),#280);
#263=STYLED_ITEM('',(#13409),#281);
#264=STYLED_ITEM('',(#13409),#282);
#265=STYLED_ITEM('',(#13409),#283);
#266=MANIFOLD_SOLID_BREP('Body1',#6843);
#267=MANIFOLD_SOLID_BREP('Body1',#6844);
#268=MANIFOLD_SOLID_BREP('Body1',#6845);
#269=MANIFOLD_SOLID_BREP('Body1',#6846);
#270=MANIFOLD_SOLID_BREP('Body1',#6847);
#271=MANIFOLD_SOLID_BREP('Body1',#6848);
#272=MANIFOLD_SOLID_BREP('Body1',#6849);
#273=MANIFOLD_SOLID_BREP('Body1',#6850);
#274=MANIFOLD_SOLID_BREP('Body1',#6851);
#275=MANIFOLD_SOLID_BREP('Body1',#6852);
#276=MANIFOLD_SOLID_BREP('Body1',#6853);
#277=MANIFOLD_SOLID_BREP('Body1',#6854);
#278=MANIFOLD_SOLID_BREP('Body1',#6855);
#279=MANIFOLD_SOLID_BREP('Body1',#6856);
#280=MANIFOLD_SOLID_BREP('Body1',#6857);
#281=MANIFOLD_SOLID_BREP('Body1',#6858);
#282=MANIFOLD_SOLID_BREP('Body1',#6859);
#283=MANIFOLD_SOLID_BREP('Body1',#6860);
#284=FACE_BOUND('',#2199,.T.);
#285=FACE_BOUND('',#2202,.T.);
#286=FACE_BOUND('',#2204,.T.);
#287=FACE_BOUND('',#2207,.T.);
#288=FACE_BOUND('',#2215,.T.);
#289=FACE_BOUND('',#2217,.T.);
#290=FACE_BOUND('',#2265,.T.);
#291=FACE_BOUND('',#2266,.T.);
#292=FACE_BOUND('',#2274,.T.);
#293=FACE_BOUND('',#2277,.T.);
#294=FACE_BOUND('',#2279,.T.);
#295=FACE_BOUND('',#2283,.T.);
#296=FACE_BOUND('',#2286,.T.);
#297=FACE_BOUND('',#2292,.T.);
#298=FACE_BOUND('',#2294,.T.);
#299=FACE_BOUND('',#2304,.T.);
#300=FACE_BOUND('',#2307,.T.);
#301=FACE_BOUND('',#2318,.T.);
#302=FACE_BOUND('',#2319,.T.);
#303=FACE_BOUND('',#2324,.T.);
#304=FACE_BOUND('',#2327,.T.);
#305=FACE_BOUND('',#2329,.T.);
#306=FACE_BOUND('',#2333,.T.);
#307=FACE_BOUND('',#2336,.T.);
#308=FACE_BOUND('',#2342,.T.);
#309=FACE_BOUND('',#2344,.T.);
#310=FACE_BOUND('',#2355,.T.);
#311=FACE_BOUND('',#2358,.T.);
#312=FACE_BOUND('',#2374,.T.);
#313=FACE_BOUND('',#2375,.T.);
#314=FACE_BOUND('',#2379,.T.);
#315=FACE_BOUND('',#2384,.T.);
#316=FACE_BOUND('',#2387,.T.);
#317=FACE_BOUND('',#2389,.T.);
#318=FACE_BOUND('',#2393,.T.);
#319=FACE_BOUND('',#2396,.T.);
#320=FACE_BOUND('',#2402,.T.);
#321=FACE_BOUND('',#2404,.T.);
#322=FACE_BOUND('',#2415,.T.);
#323=FACE_BOUND('',#2418,.T.);
#324=FACE_BOUND('',#2433,.T.);
#325=FACE_BOUND('',#2435,.T.);
#326=FACE_BOUND('',#2437,.T.);
#327=FACE_BOUND('',#2440,.T.);
#328=FACE_BOUND('',#2448,.T.);
#329=FACE_BOUND('',#2451,.T.);
#330=FACE_BOUND('',#2454,.T.);
#331=FACE_BOUND('',#2460,.T.);
#332=FACE_BOUND('',#2462,.T.);
#333=FACE_BOUND('',#2464,.T.);
#334=FACE_BOUND('',#2467,.T.);
#335=FACE_BOUND('',#2475,.T.);
#336=FACE_BOUND('',#2478,.T.);
#337=FACE_BOUND('',#2481,.T.);
#338=FACE_BOUND('',#2487,.T.);
#339=FACE_BOUND('',#2489,.T.);
#340=FACE_BOUND('',#2491,.T.);
#341=FACE_BOUND('',#2494,.T.);
#342=FACE_BOUND('',#2502,.T.);
#343=FACE_BOUND('',#2505,.T.);
#344=FACE_BOUND('',#2508,.T.);
#345=FACE_BOUND('',#2515,.T.);
#346=FACE_BOUND('',#2518,.T.);
#347=FACE_BOUND('',#2525,.T.);
#348=FACE_BOUND('',#2527,.T.);
#349=FACE_BOUND('',#2535,.T.);
#350=FACE_BOUND('',#2536,.T.);
#351=FACE_BOUND('',#2538,.T.);
#352=FACE_BOUND('',#2542,.T.);
#353=FACE_BOUND('',#2545,.T.);
#354=FACE_BOUND('',#2551,.T.);
#355=FACE_BOUND('',#2552,.T.);
#356=FACE_BOUND('',#2556,.T.);
#357=FACE_BOUND('',#2559,.T.);
#358=FACE_BOUND('',#2562,.T.);
#359=FACE_BOUND('',#2565,.T.);
#360=FACE_BOUND('',#2574,.T.);
#361=FACE_BOUND('',#2576,.T.);
#362=FACE_BOUND('',#2584,.T.);
#363=FACE_BOUND('',#2585,.T.);
#364=FACE_BOUND('',#2590,.T.);
#365=FACE_BOUND('',#2592,.T.);
#366=FACE_BOUND('',#2599,.T.);
#367=FACE_BOUND('',#2601,.T.);
#368=FACE_BOUND('',#2609,.T.);
#369=FACE_BOUND('',#2610,.T.);
#370=FACE_BOUND('',#2620,.T.);
#371=FACE_BOUND('',#2622,.T.);
#372=FACE_BOUND('',#2626,.T.);
#373=FACE_BOUND('',#2629,.T.);
#374=FACE_BOUND('',#2636,.T.);
#375=FACE_BOUND('',#2638,.T.);
#376=FACE_BOUND('',#2658,.T.);
#377=FACE_BOUND('',#2660,.T.);
#378=FACE_BOUND('',#2662,.T.);
#379=FACE_BOUND('',#2665,.T.);
#380=FACE_BOUND('',#2673,.T.);
#381=FACE_BOUND('',#2676,.T.);
#382=FACE_BOUND('',#2679,.T.);
#383=ELLIPSE('',#7086,20.7055236081625,19.9999999999245);
#384=ELLIPSE('',#7091,77.2740661068614,20.0000000018389);
#385=ELLIPSE('',#7093,20.7055236081649,19.9999999999297);
#386=ELLIPSE('',#7096,77.2740661044132,20.0000000006464);
#387=ELLIPSE('',#7195,3.65324790347504,2.58323636587766);
#388=ELLIPSE('',#7196,3.65324790353112,2.58323636594297);
#389=ELLIPSE('',#7197,3.65324790353033,2.58323636594184);
#390=ELLIPSE('',#7198,3.65324790353218,2.58323636594453);
#391=ELLIPSE('',#7199,3.65324790349574,2.58323636589973);
#392=ELLIPSE('',#7706,4.01857269385652,2.84156000250712);
#393=ELLIPSE('',#7707,4.01857269388513,2.84156000253857);
#394=ELLIPSE('',#7708,4.01857269388335,2.841560002536);
#395=ELLIPSE('',#7709,4.01857269388599,2.84156000253982);
#396=ELLIPSE('',#7710,4.01857269402875,2.84156000270659);
#397=PLANE('',#7085);
#398=PLANE('',#7087);
#399=PLANE('',#7092);
#400=PLANE('',#7094);
#401=PLANE('',#7104);
#402=PLANE('',#7106);
#403=PLANE('',#7107);
#404=PLANE('',#7108);
#405=PLANE('',#7109);
#406=PLANE('',#7110);
#407=PLANE('',#7114);
#408=PLANE('',#7118);
#409=PLANE('',#7120);
#410=PLANE('',#7122);
#411=PLANE('',#7123);
#412=PLANE('',#7125);
#413=PLANE('',#7126);
#414=PLANE('',#7188);
#415=PLANE('',#7189);
#416=PLANE('',#7220);
#417=PLANE('',#7221);
#418=PLANE('',#7223);
#419=PLANE('',#7225);
#420=PLANE('',#7234);
#421=PLANE('',#7235);
#422=PLANE('',#7236);
#423=PLANE('',#7237);
#424=PLANE('',#7238);
#425=PLANE('',#7239);
#426=PLANE('',#7242);
#427=PLANE('',#7243);
#428=PLANE('',#7246);
#429=PLANE('',#7247);
#430=PLANE('',#7248);
#431=PLANE('',#7249);
#432=PLANE('',#7250);
#433=PLANE('',#7253);
#434=PLANE('',#7256);
#435=PLANE('',#7257);
#436=PLANE('',#7263);
#437=PLANE('',#7264);
#438=PLANE('',#7267);
#439=PLANE('',#7268);
#440=PLANE('',#7271);
#441=PLANE('',#7298);
#442=PLANE('',#7304);
#443=PLANE('',#7306);
#444=PLANE('',#7309);
#445=PLANE('',#7312);
#446=PLANE('',#7313);
#447=PLANE('',#7314);
#448=PLANE('',#7317);
#449=PLANE('',#7318);
#450=PLANE('',#7321);
#451=PLANE('',#7322);
#452=PLANE('',#7323);
#453=PLANE('',#7324);
#454=PLANE('',#7325);
#455=PLANE('',#7330);
#456=PLANE('',#7335);
#457=PLANE('',#7336);
#458=PLANE('',#7343);
#459=PLANE('',#7344);
#460=PLANE('',#7347);
#461=PLANE('',#7348);
#462=PLANE('',#7351);
#463=PLANE('',#7389);
#464=PLANE('',#7395);
#465=PLANE('',#7396);
#466=PLANE('',#7400);
#467=PLANE('',#7404);
#468=PLANE('',#7405);
#469=PLANE('',#7406);
#470=PLANE('',#7409);
#471=PLANE('',#7410);
#472=PLANE('',#7413);
#473=PLANE('',#7414);
#474=PLANE('',#7415);
#475=PLANE('',#7416);
#476=PLANE('',#7417);
#477=PLANE('',#7422);
#478=PLANE('',#7427);
#479=PLANE('',#7428);
#480=PLANE('',#7435);
#481=PLANE('',#7436);
#482=PLANE('',#7439);
#483=PLANE('',#7440);
#484=PLANE('',#7443);
#485=PLANE('',#7464);
#486=PLANE('',#7465);
#487=PLANE('',#7466);
#488=PLANE('',#7468);
#489=PLANE('',#7469);
#490=PLANE('',#7471);
#491=PLANE('',#7473);
#492=PLANE('',#7484);
#493=PLANE('',#7485);
#494=PLANE('',#7486);
#495=PLANE('',#7487);
#496=PLANE('',#7488);
#497=PLANE('',#7489);
#498=PLANE('',#7503);
#499=PLANE('',#7504);
#500=PLANE('',#7505);
#501=PLANE('',#7507);
#502=PLANE('',#7508);
#503=PLANE('',#7510);
#504=PLANE('',#7512);
#505=PLANE('',#7523);
#506=PLANE('',#7524);
#507=PLANE('',#7525);
#508=PLANE('',#7526);
#509=PLANE('',#7527);
#510=PLANE('',#7528);
#511=PLANE('',#7542);
#512=PLANE('',#7543);
#513=PLANE('',#7544);
#514=PLANE('',#7546);
#515=PLANE('',#7547);
#516=PLANE('',#7549);
#517=PLANE('',#7551);
#518=PLANE('',#7562);
#519=PLANE('',#7563);
#520=PLANE('',#7564);
#521=PLANE('',#7565);
#522=PLANE('',#7566);
#523=PLANE('',#7567);
#524=PLANE('',#7578);
#525=PLANE('',#7579);
#526=PLANE('',#7580);
#527=PLANE('',#7581);
#528=PLANE('',#7582);
#529=PLANE('',#7583);
#530=PLANE('',#7584);
#531=PLANE('',#7585);
#532=PLANE('',#7586);
#533=PLANE('',#7587);
#534=PLANE('',#7588);
#535=PLANE('',#7589);
#536=PLANE('',#7590);
#537=PLANE('',#7591);
#538=PLANE('',#7605);
#539=PLANE('',#7606);
#540=PLANE('',#7607);
#541=PLANE('',#7608);
#542=PLANE('',#7609);
#543=PLANE('',#7648);
#544=PLANE('',#7649);
#545=PLANE('',#7650);
#546=PLANE('',#7651);
#547=PLANE('',#7652);
#548=PLANE('',#7653);
#549=PLANE('',#7654);
#550=PLANE('',#7655);
#551=PLANE('',#7656);
#552=PLANE('',#7657);
#553=PLANE('',#7658);
#554=PLANE('',#7659);
#555=PLANE('',#7660);
#556=PLANE('',#7661);
#557=PLANE('',#7662);
#558=PLANE('',#7663);
#559=PLANE('',#7664);
#560=PLANE('',#7665);
#561=PLANE('',#7674);
#562=PLANE('',#7686);
#563=PLANE('',#7687);
#564=PLANE('',#7691);
#565=PLANE('',#7692);
#566=PLANE('',#7693);
#567=PLANE('',#7694);
#568=PLANE('',#7695);
#569=PLANE('',#7696);
#570=PLANE('',#7697);
#571=PLANE('',#7698);
#572=PLANE('',#7699);
#573=PLANE('',#7723);
#574=PLANE('',#7724);
#575=PLANE('',#7726);
#576=PLANE('',#7728);
#577=PLANE('',#7735);
#578=PLANE('',#7736);
#579=PLANE('',#7737);
#580=PLANE('',#7740);
#581=PLANE('',#7743);
#582=PLANE('',#7744);
#583=PLANE('',#7746);
#584=PLANE('',#7749);
#585=PLANE('',#7750);
#586=PLANE('',#7754);
#587=PLANE('',#7755);
#588=PLANE('',#7756);
#589=PLANE('',#7757);
#590=PLANE('',#7758);
#591=PLANE('',#7761);
#592=PLANE('',#7764);
#593=PLANE('',#7765);
#594=PLANE('',#7772);
#595=PLANE('',#7773);
#596=PLANE('',#7781);
#597=PLANE('',#7793);
#598=PLANE('',#7794);
#599=PLANE('',#7795);
#600=PLANE('',#7797);
#601=PLANE('',#7798);
#602=PLANE('',#7800);
#603=PLANE('',#7802);
#604=PLANE('',#7813);
#605=PLANE('',#7814);
#606=PLANE('',#7815);
#607=PLANE('',#7816);
#608=PLANE('',#7817);
#609=PLANE('',#7818);
#610=LINE('',#9916,#1128);
#611=LINE('',#9922,#1129);
#612=LINE('',#9928,#1130);
#613=LINE('',#9930,#1131);
#614=LINE('',#9934,#1132);
#615=LINE('',#9936,#1133);
#616=LINE('',#9938,#1134);
#617=LINE('',#9943,#1135);
#618=LINE('',#9947,#1136);
#619=LINE('',#9951,#1137);
#620=LINE('',#9957,#1138);
#621=LINE('',#9958,#1139);
#622=LINE('',#9963,#1140);
#623=LINE('',#9969,#1141);
#624=LINE('',#9975,#1142);
#625=LINE('',#9978,#1143);
#626=LINE('',#9981,#1144);
#627=LINE('',#9985,#1145);
#628=LINE('',#9990,#1146);
#629=LINE('',#9992,#1147);
#630=LINE('',#9994,#1148);
#631=LINE('',#9995,#1149);
#632=LINE('',#9997,#1150);
#633=LINE('',#10001,#1151);
#634=LINE('',#10003,#1152);
#635=LINE('',#10005,#1153);
#636=LINE('',#10006,#1154);
#637=LINE('',#10010,#1155);
#638=LINE('',#10012,#1156);
#639=LINE('',#10014,#1157);
#640=LINE('',#10015,#1158);
#641=LINE('',#10019,#1159);
#642=LINE('',#10021,#1160);
#643=LINE('',#10023,#1161);
#644=LINE('',#10024,#1162);
#645=LINE('',#10028,#1163);
#646=LINE('',#10030,#1164);
#647=LINE('',#10031,#1165);
#648=LINE('',#10032,#1166);
#649=LINE('',#10041,#1167);
#650=LINE('',#10043,#1168);
#651=LINE('',#10045,#1169);
#652=LINE('',#10046,#1170);
#653=LINE('',#10054,#1171);
#654=LINE('',#10056,#1172);
#655=LINE('',#10058,#1173);
#656=LINE('',#10059,#1174);
#657=LINE('',#10062,#1175);
#658=LINE('',#10065,#1176);
#659=LINE('',#10067,#1177);
#660=LINE('',#10068,#1178);
#661=LINE('',#10071,#1179);
#662=LINE('',#10074,#1180);
#663=LINE('',#10076,#1181);
#664=LINE('',#10077,#1182);
#665=LINE('',#10079,#1183);
#666=LINE('',#10081,#1184);
#667=LINE('',#10084,#1185);
#668=LINE('',#10147,#1186);
#669=LINE('',#10148,#1187);
#670=LINE('',#10150,#1188);
#671=LINE('',#10152,#1189);
#672=LINE('',#10181,#1190);
#673=LINE('',#10185,#1191);
#674=LINE('',#10189,#1192);
#675=LINE('',#10193,#1193);
#676=LINE('',#10199,#1194);
#677=LINE('',#10205,#1195);
#678=LINE('',#10211,#1196);
#679=LINE('',#10217,#1197);
#680=LINE('',#10223,#1198);
#681=LINE('',#10284,#1199);
#682=LINE('',#10344,#1200);
#683=LINE('',#10433,#1201);
#684=LINE('',#10434,#1202);
#685=LINE('',#10437,#1203);
#686=LINE('',#10441,#1204);
#687=LINE('',#10443,#1205);
#688=LINE('',#10448,#1206);
#689=LINE('',#10450,#1207);
#690=LINE('',#10452,#1208);
#691=LINE('',#10453,#1209);
#692=LINE('',#10469,#1210);
#693=LINE('',#10475,#1211);
#694=LINE('',#10479,#1212);
#695=LINE('',#10483,#1213);
#696=LINE('',#10485,#1214);
#697=LINE('',#10486,#1215);
#698=LINE('',#10488,#1216);
#699=LINE('',#10490,#1217);
#700=LINE('',#10494,#1218);
#701=LINE('',#10496,#1219);
#702=LINE('',#10497,#1220);
#703=LINE('',#10501,#1221);
#704=LINE('',#10505,#1222);
#705=LINE('',#10506,#1223);
#706=LINE('',#10508,#1224);
#707=LINE('',#10512,#1225);
#708=LINE('',#10513,#1226);
#709=LINE('',#10516,#1227);
#710=LINE('',#10520,#1228);
#711=LINE('',#10523,#1229);
#712=LINE('',#10524,#1230);
#713=LINE('',#10526,#1231);
#714=LINE('',#10527,#1232);
#715=LINE('',#10528,#1233);
#716=LINE('',#10531,#1234);
#717=LINE('',#10533,#1235);
#718=LINE('',#10534,#1236);
#719=LINE('',#10535,#1237);
#720=LINE('',#10539,#1238);
#721=LINE('',#10540,#1239);
#722=LINE('',#10541,#1240);
#723=LINE('',#10543,#1241);
#724=LINE('',#10560,#1242);
#725=LINE('',#10562,#1243);
#726=LINE('',#10564,#1244);
#727=LINE('',#10565,#1245);
#728=LINE('',#10568,#1246);
#729=LINE('',#10572,#1247);
#730=LINE('',#10575,#1248);
#731=LINE('',#10576,#1249);
#732=LINE('',#10580,#1250);
#733=LINE('',#10583,#1251);
#734=LINE('',#10591,#1252);
#735=LINE('',#10597,#1253);
#736=LINE('',#10603,#1254);
#737=LINE('',#10609,#1255);
#738=LINE('',#10615,#1256);
#739=LINE('',#10676,#1257);
#740=LINE('',#10750,#1258);
#741=LINE('',#10847,#1259);
#742=LINE('',#10859,#1260);
#743=LINE('',#10862,#1261);
#744=LINE('',#10866,#1262);
#745=LINE('',#10868,#1263);
#746=LINE('',#10870,#1264);
#747=LINE('',#10871,#1265);
#748=LINE('',#10877,#1266);
#749=LINE('',#10881,#1267);
#750=LINE('',#10888,#1268);
#751=LINE('',#10890,#1269);
#752=LINE('',#10891,#1270);
#753=LINE('',#10896,#1271);
#754=LINE('',#10927,#1272);
#755=LINE('',#10931,#1273);
#756=LINE('',#10933,#1274);
#757=LINE('',#10934,#1275);
#758=LINE('',#10938,#1276);
#759=LINE('',#10942,#1277);
#760=LINE('',#10943,#1278);
#761=LINE('',#10945,#1279);
#762=LINE('',#10949,#1280);
#763=LINE('',#10950,#1281);
#764=LINE('',#10953,#1282);
#765=LINE('',#10957,#1283);
#766=LINE('',#10960,#1284);
#767=LINE('',#10962,#1285);
#768=LINE('',#10964,#1286);
#769=LINE('',#10966,#1287);
#770=LINE('',#10967,#1288);
#771=LINE('',#10971,#1289);
#772=LINE('',#10973,#1290);
#773=LINE('',#10975,#1291);
#774=LINE('',#10976,#1292);
#775=LINE('',#10977,#1293);
#776=LINE('',#10981,#1294);
#777=LINE('',#10982,#1295);
#778=LINE('',#10983,#1296);
#779=LINE('',#10987,#1297);
#780=LINE('',#10989,#1298);
#781=LINE('',#10991,#1299);
#782=LINE('',#10992,#1300);
#783=LINE('',#11014,#1301);
#784=LINE('',#11016,#1302);
#785=LINE('',#11018,#1303);
#786=LINE('',#11019,#1304);
#787=LINE('',#11022,#1305);
#788=LINE('',#11026,#1306);
#789=LINE('',#11029,#1307);
#790=LINE('',#11030,#1308);
#791=LINE('',#11034,#1309);
#792=LINE('',#11037,#1310);
#793=LINE('',#11041,#1311);
#794=LINE('',#11043,#1312);
#795=LINE('',#11052,#1313);
#796=LINE('',#11058,#1314);
#797=LINE('',#11064,#1315);
#798=LINE('',#11070,#1316);
#799=LINE('',#11076,#1317);
#800=LINE('',#11137,#1318);
#801=LINE('',#11221,#1319);
#802=LINE('',#11318,#1320);
#803=LINE('',#11321,#1321);
#804=LINE('',#11326,#1322);
#805=LINE('',#11327,#1323);
#806=LINE('',#11415,#1324);
#807=LINE('',#11423,#1325);
#808=LINE('',#11426,#1326);
#809=LINE('',#11430,#1327);
#810=LINE('',#11432,#1328);
#811=LINE('',#11434,#1329);
#812=LINE('',#11435,#1330);
#813=LINE('',#11441,#1331);
#814=LINE('',#11445,#1332);
#815=LINE('',#11449,#1333);
#816=LINE('',#11451,#1334);
#817=LINE('',#11452,#1335);
#818=LINE('',#11458,#1336);
#819=LINE('',#11463,#1337);
#820=LINE('',#11468,#1338);
#821=LINE('',#11470,#1339);
#822=LINE('',#11471,#1340);
#823=LINE('',#11475,#1341);
#824=LINE('',#11479,#1342);
#825=LINE('',#11480,#1343);
#826=LINE('',#11482,#1344);
#827=LINE('',#11486,#1345);
#828=LINE('',#11487,#1346);
#829=LINE('',#11490,#1347);
#830=LINE('',#11494,#1348);
#831=LINE('',#11497,#1349);
#832=LINE('',#11499,#1350);
#833=LINE('',#11501,#1351);
#834=LINE('',#11503,#1352);
#835=LINE('',#11504,#1353);
#836=LINE('',#11508,#1354);
#837=LINE('',#11510,#1355);
#838=LINE('',#11512,#1356);
#839=LINE('',#11513,#1357);
#840=LINE('',#11514,#1358);
#841=LINE('',#11518,#1359);
#842=LINE('',#11519,#1360);
#843=LINE('',#11520,#1361);
#844=LINE('',#11524,#1362);
#845=LINE('',#11526,#1363);
#846=LINE('',#11528,#1364);
#847=LINE('',#11529,#1365);
#848=LINE('',#11551,#1366);
#849=LINE('',#11553,#1367);
#850=LINE('',#11555,#1368);
#851=LINE('',#11556,#1369);
#852=LINE('',#11559,#1370);
#853=LINE('',#11563,#1371);
#854=LINE('',#11566,#1372);
#855=LINE('',#11567,#1373);
#856=LINE('',#11571,#1374);
#857=LINE('',#11574,#1375);
#858=LINE('',#11581,#1376);
#859=LINE('',#11583,#1377);
#860=LINE('',#11592,#1378);
#861=LINE('',#11598,#1379);
#862=LINE('',#11604,#1380);
#863=LINE('',#11609,#1381);
#864=LINE('',#11611,#1382);
#865=LINE('',#11613,#1383);
#866=LINE('',#11614,#1384);
#867=LINE('',#11620,#1385);
#868=LINE('',#11621,#1386);
#869=LINE('',#11624,#1387);
#870=LINE('',#11625,#1388);
#871=LINE('',#11628,#1389);
#872=LINE('',#11631,#1390);
#873=LINE('',#11639,#1391);
#874=LINE('',#11646,#1392);
#875=LINE('',#11649,#1393);
#876=LINE('',#11654,#1394);
#877=LINE('',#11659,#1395);
#878=LINE('',#11661,#1396);
#879=LINE('',#11663,#1397);
#880=LINE('',#11664,#1398);
#881=LINE('',#11667,#1399);
#882=LINE('',#11668,#1400);
#883=LINE('',#11670,#1401);
#884=LINE('',#11672,#1402);
#885=LINE('',#11682,#1403);
#886=LINE('',#11688,#1404);
#887=LINE('',#11694,#1405);
#888=LINE('',#11699,#1406);
#889=LINE('',#11701,#1407);
#890=LINE('',#11703,#1408);
#891=LINE('',#11704,#1409);
#892=LINE('',#11710,#1410);
#893=LINE('',#11711,#1411);
#894=LINE('',#11714,#1412);
#895=LINE('',#11715,#1413);
#896=LINE('',#11718,#1414);
#897=LINE('',#11721,#1415);
#898=LINE('',#11729,#1416);
#899=LINE('',#11736,#1417);
#900=LINE('',#11739,#1418);
#901=LINE('',#11744,#1419);
#902=LINE('',#11749,#1420);
#903=LINE('',#11751,#1421);
#904=LINE('',#11753,#1422);
#905=LINE('',#11754,#1423);
#906=LINE('',#11757,#1424);
#907=LINE('',#11758,#1425);
#908=LINE('',#11760,#1426);
#909=LINE('',#11762,#1427);
#910=LINE('',#11772,#1428);
#911=LINE('',#11778,#1429);
#912=LINE('',#11784,#1430);
#913=LINE('',#11789,#1431);
#914=LINE('',#11791,#1432);
#915=LINE('',#11793,#1433);
#916=LINE('',#11794,#1434);
#917=LINE('',#11800,#1435);
#918=LINE('',#11801,#1436);
#919=LINE('',#11804,#1437);
#920=LINE('',#11805,#1438);
#921=LINE('',#11808,#1439);
#922=LINE('',#11811,#1440);
#923=LINE('',#11819,#1441);
#924=LINE('',#11826,#1442);
#925=LINE('',#11829,#1443);
#926=LINE('',#11834,#1444);
#927=LINE('',#11839,#1445);
#928=LINE('',#11841,#1446);
#929=LINE('',#11843,#1447);
#930=LINE('',#11844,#1448);
#931=LINE('',#11847,#1449);
#932=LINE('',#11848,#1450);
#933=LINE('',#11850,#1451);
#934=LINE('',#11852,#1452);
#935=LINE('',#11859,#1453);
#936=LINE('',#11865,#1454);
#937=LINE('',#11871,#1455);
#938=LINE('',#11876,#1456);
#939=LINE('',#11878,#1457);
#940=LINE('',#11880,#1458);
#941=LINE('',#11881,#1459);
#942=LINE('',#11885,#1460);
#943=LINE('',#11887,#1461);
#944=LINE('',#11888,#1462);
#945=LINE('',#11890,#1463);
#946=LINE('',#11891,#1464);
#947=LINE('',#11894,#1465);
#948=LINE('',#11896,#1466);
#949=LINE('',#11897,#1467);
#950=LINE('',#11900,#1468);
#951=LINE('',#11902,#1469);
#952=LINE('',#11904,#1470);
#953=LINE('',#11906,#1471);
#954=LINE('',#11907,#1472);
#955=LINE('',#11909,#1473);
#956=LINE('',#11910,#1474);
#957=LINE('',#11914,#1475);
#958=LINE('',#11916,#1476);
#959=LINE('',#11918,#1477);
#960=LINE('',#11919,#1478);
#961=LINE('',#11923,#1479);
#962=LINE('',#11924,#1480);
#963=LINE('',#11926,#1481);
#964=LINE('',#11927,#1482);
#965=LINE('',#11929,#1483);
#966=LINE('',#11931,#1484);
#967=LINE('',#11933,#1485);
#968=LINE('',#11945,#1486);
#969=LINE('',#12017,#1487);
#970=LINE('',#12147,#1488);
#971=LINE('',#12150,#1489);
#972=LINE('',#12154,#1490);
#973=LINE('',#12156,#1491);
#974=LINE('',#12158,#1492);
#975=LINE('',#12159,#1493);
#976=LINE('',#12161,#1494);
#977=LINE('',#12162,#1495);
#978=LINE('',#12164,#1496);
#979=LINE('',#12166,#1497);
#980=LINE('',#12181,#1498);
#981=LINE('',#12187,#1499);
#982=LINE('',#12193,#1500);
#983=LINE('',#12199,#1501);
#984=LINE('',#12235,#1502);
#985=LINE('',#12237,#1503);
#986=LINE('',#12239,#1504);
#987=LINE('',#12240,#1505);
#988=LINE('',#12243,#1506);
#989=LINE('',#12245,#1507);
#990=LINE('',#12246,#1508);
#991=LINE('',#12249,#1509);
#992=LINE('',#12250,#1510);
#993=LINE('',#12253,#1511);
#994=LINE('',#12254,#1512);
#995=LINE('',#12256,#1513);
#996=LINE('',#12260,#1514);
#997=LINE('',#12261,#1515);
#998=LINE('',#12264,#1516);
#999=LINE('',#12265,#1517);
#1000=LINE('',#12267,#1518);
#1001=LINE('',#12272,#1519);
#1002=LINE('',#12273,#1520);
#1003=LINE('',#12274,#1521);
#1004=LINE('',#12276,#1522);
#1005=LINE('',#12278,#1523);
#1006=LINE('',#12279,#1524);
#1007=LINE('',#12282,#1525);
#1008=LINE('',#12283,#1526);
#1009=LINE('',#12286,#1527);
#1010=LINE('',#12288,#1528);
#1011=LINE('',#12290,#1529);
#1012=LINE('',#12291,#1530);
#1013=LINE('',#12292,#1531);
#1014=LINE('',#12295,#1532);
#1015=LINE('',#12297,#1533);
#1016=LINE('',#12298,#1534);
#1017=LINE('',#12306,#1535);
#1018=LINE('',#12312,#1536);
#1019=LINE('',#12373,#1537);
#1020=LINE('',#12397,#1538);
#1021=LINE('',#12399,#1539);
#1022=LINE('',#12401,#1540);
#1023=LINE('',#12406,#1541);
#1024=LINE('',#12424,#1542);
#1025=LINE('',#12441,#1543);
#1026=LINE('',#12447,#1544);
#1027=LINE('',#12451,#1545);
#1028=LINE('',#12551,#1546);
#1029=LINE('',#12553,#1547);
#1030=LINE('',#12557,#1548);
#1031=LINE('',#12562,#1549);
#1032=LINE('',#12563,#1550);
#1033=LINE('',#12566,#1551);
#1034=LINE('',#12567,#1552);
#1035=LINE('',#12569,#1553);
#1036=LINE('',#12573,#1554);
#1037=LINE('',#12575,#1555);
#1038=LINE('',#12576,#1556);
#1039=LINE('',#12579,#1557);
#1040=LINE('',#12581,#1558);
#1041=LINE('',#12582,#1559);
#1042=LINE('',#12584,#1560);
#1043=LINE('',#12585,#1561);
#1044=LINE('',#12593,#1562);
#1045=LINE('',#12660,#1563);
#1046=LINE('',#12707,#1564);
#1047=LINE('',#12711,#1565);
#1048=LINE('',#12715,#1566);
#1049=LINE('',#12719,#1567);
#1050=LINE('',#12725,#1568);
#1051=LINE('',#12731,#1569);
#1052=LINE('',#12737,#1570);
#1053=LINE('',#12838,#1571);
#1054=LINE('',#12839,#1572);
#1055=LINE('',#12842,#1573);
#1056=LINE('',#12846,#1574);
#1057=LINE('',#12848,#1575);
#1058=LINE('',#12853,#1576);
#1059=LINE('',#12855,#1577);
#1060=LINE('',#12857,#1578);
#1061=LINE('',#12858,#1579);
#1062=LINE('',#12876,#1580);
#1063=LINE('',#12879,#1581);
#1064=LINE('',#12882,#1582);
#1065=LINE('',#12884,#1583);
#1066=LINE('',#12885,#1584);
#1067=LINE('',#12893,#1585);
#1068=LINE('',#12895,#1586);
#1069=LINE('',#12896,#1587);
#1070=LINE('',#12903,#1588);
#1071=LINE('',#12905,#1589);
#1072=LINE('',#12906,#1590);
#1073=LINE('',#12908,#1591);
#1074=LINE('',#12913,#1592);
#1075=LINE('',#12915,#1593);
#1076=LINE('',#12916,#1594);
#1077=LINE('',#12920,#1595);
#1078=LINE('',#12924,#1596);
#1079=LINE('',#12925,#1597);
#1080=LINE('',#12927,#1598);
#1081=LINE('',#12931,#1599);
#1082=LINE('',#12932,#1600);
#1083=LINE('',#12935,#1601);
#1084=LINE('',#12939,#1602);
#1085=LINE('',#12940,#1603);
#1086=LINE('',#12944,#1604);
#1087=LINE('',#12945,#1605);
#1088=LINE('',#12947,#1606);
#1089=LINE('',#12948,#1607);
#1090=LINE('',#12949,#1608);
#1091=LINE('',#12952,#1609);
#1092=LINE('',#12954,#1610);
#1093=LINE('',#12955,#1611);
#1094=LINE('',#12956,#1612);
#1095=LINE('',#12960,#1613);
#1096=LINE('',#12961,#1614);
#1097=LINE('',#12962,#1615);
#1098=LINE('',#12964,#1616);
#1099=LINE('',#12979,#1617);
#1100=LINE('',#12980,#1618);
#1101=LINE('',#12981,#1619);
#1102=LINE('',#12983,#1620);
#1103=LINE('',#13056,#1621);
#1104=LINE('',#13062,#1622);
#1105=LINE('',#13068,#1623);
#1106=LINE('',#13073,#1624);
#1107=LINE('',#13075,#1625);
#1108=LINE('',#13077,#1626);
#1109=LINE('',#13078,#1627);
#1110=LINE('',#13084,#1628);
#1111=LINE('',#13085,#1629);
#1112=LINE('',#13088,#1630);
#1113=LINE('',#13089,#1631);
#1114=LINE('',#13092,#1632);
#1115=LINE('',#13095,#1633);
#1116=LINE('',#13103,#1634);
#1117=LINE('',#13110,#1635);
#1118=LINE('',#13113,#1636);
#1119=LINE('',#13118,#1637);
#1120=LINE('',#13123,#1638);
#1121=LINE('',#13125,#1639);
#1122=LINE('',#13127,#1640);
#1123=LINE('',#13128,#1641);
#1124=LINE('',#13131,#1642);
#1125=LINE('',#13132,#1643);
#1126=LINE('',#13134,#1644);
#1127=LINE('',#13136,#1645);
#1128=VECTOR('',#7865,1.5);
#1129=VECTOR('',#7872,1.5);
#1130=VECTOR('',#7879,1000.);
#1131=VECTOR('',#7882,1000.);
#1132=VECTOR('',#7885,1000.);
#1133=VECTOR('',#7886,1000.);
#1134=VECTOR('',#7887,1000.);
#1135=VECTOR('',#7892,1000.);
#1136=VECTOR('',#7895,1000.);
#1137=VECTOR('',#7898,1000.);
#1138=VECTOR('',#7905,1000.);
#1139=VECTOR('',#7906,1000.);
#1140=VECTOR('',#7911,1000.);
#1141=VECTOR('',#7918,1000.);
#1142=VECTOR('',#7925,1000.);
#1143=VECTOR('',#7928,1000.);
#1144=VECTOR('',#7929,1000.);
#1145=VECTOR('',#7932,1000.);
#1146=VECTOR('',#7937,1000.);
#1147=VECTOR('',#7938,1000.);
#1148=VECTOR('',#7939,1000.);
#1149=VECTOR('',#7940,1000.);
#1150=VECTOR('',#7943,1000.);
#1151=VECTOR('',#7946,1000.);
#1152=VECTOR('',#7947,1000.);
#1153=VECTOR('',#7948,1000.);
#1154=VECTOR('',#7949,1000.);
#1155=VECTOR('',#7952,1000.);
#1156=VECTOR('',#7953,1000.);
#1157=VECTOR('',#7954,1000.);
#1158=VECTOR('',#7955,1000.);
#1159=VECTOR('',#7958,1000.);
#1160=VECTOR('',#7959,1000.);
#1161=VECTOR('',#7960,1000.);
#1162=VECTOR('',#7961,1000.);
#1163=VECTOR('',#7964,1000.);
#1164=VECTOR('',#7965,1000.);
#1165=VECTOR('',#7966,1000.);
#1166=VECTOR('',#7967,1000.);
#1167=VECTOR('',#7976,1000.);
#1168=VECTOR('',#7977,1000.);
#1169=VECTOR('',#7978,1000.);
#1170=VECTOR('',#7979,1000.);
#1171=VECTOR('',#7988,1000.);
#1172=VECTOR('',#7989,1000.);
#1173=VECTOR('',#7990,1000.);
#1174=VECTOR('',#7991,1000.);
#1175=VECTOR('',#7994,1000.);
#1176=VECTOR('',#7997,1000.);
#1177=VECTOR('',#7998,1000.);
#1178=VECTOR('',#7999,1000.);
#1179=VECTOR('',#8002,1000.);
#1180=VECTOR('',#8005,1000.);
#1181=VECTOR('',#8006,1000.);
#1182=VECTOR('',#8007,1000.);
#1183=VECTOR('',#8010,1000.);
#1184=VECTOR('',#8013,1000.);
#1185=VECTOR('',#8018,1000.);
#1186=VECTOR('',#8143,1000.);
#1187=VECTOR('',#8144,1000.);
#1188=VECTOR('',#8147,1000.);
#1189=VECTOR('',#8150,1000.);
#1190=VECTOR('',#8163,1000.);
#1191=VECTOR('',#8166,1000.);
#1192=VECTOR('',#8169,1000.);
#1193=VECTOR('',#8172,1000.);
#1194=VECTOR('',#8179,1.5);
#1195=VECTOR('',#8186,1.);
#1196=VECTOR('',#8193,1.);
#1197=VECTOR('',#8200,1.);
#1198=VECTOR('',#8207,1.5);
#1199=VECTOR('',#8210,1.5);
#1200=VECTOR('',#8219,13.);
#1201=VECTOR('',#8224,1000.);
#1202=VECTOR('',#8225,1000.);
#1203=VECTOR('',#8228,1000.);
#1204=VECTOR('',#8233,1000.);
#1205=VECTOR('',#8234,1000.);
#1206=VECTOR('',#8239,1000.);
#1207=VECTOR('',#8240,1000.);
#1208=VECTOR('',#8241,1000.);
#1209=VECTOR('',#8242,1000.);
#1210=VECTOR('',#8249,1000.);
#1211=VECTOR('',#8256,1000.);
#1212=VECTOR('',#8259,1000.);
#1213=VECTOR('',#8264,1000.);
#1214=VECTOR('',#8265,1000.);
#1215=VECTOR('',#8266,1000.);
#1216=VECTOR('',#8269,1000.);
#1217=VECTOR('',#8272,1000.);
#1218=VECTOR('',#8277,1000.);
#1219=VECTOR('',#8278,1000.);
#1220=VECTOR('',#8279,1000.);
#1221=VECTOR('',#8282,1000.);
#1222=VECTOR('',#8285,1000.);
#1223=VECTOR('',#8286,1000.);
#1224=VECTOR('',#8287,1000.);
#1225=VECTOR('',#8292,1000.);
#1226=VECTOR('',#8293,1000.);
#1227=VECTOR('',#8296,1000.);
#1228=VECTOR('',#8301,1000.);
#1229=VECTOR('',#8304,1000.);
#1230=VECTOR('',#8305,1000.);
#1231=VECTOR('',#8306,1000.);
#1232=VECTOR('',#8307,1000.);
#1233=VECTOR('',#8308,1000.);
#1234=VECTOR('',#8311,1000.);
#1235=VECTOR('',#8312,1000.);
#1236=VECTOR('',#8313,1000.);
#1237=VECTOR('',#8314,1000.);
#1238=VECTOR('',#8317,1000.);
#1239=VECTOR('',#8318,1000.);
#1240=VECTOR('',#8319,1000.);
#1241=VECTOR('',#8322,1000.);
#1242=VECTOR('',#8351,1000.);
#1243=VECTOR('',#8352,1000.);
#1244=VECTOR('',#8353,1000.);
#1245=VECTOR('',#8354,1000.);
#1246=VECTOR('',#8357,1000.);
#1247=VECTOR('',#8362,1000.);
#1248=VECTOR('',#8365,1000.);
#1249=VECTOR('',#8366,1000.);
#1250=VECTOR('',#8371,1000.);
#1251=VECTOR('',#8376,1000.);
#1252=VECTOR('',#8387,1.35);
#1253=VECTOR('',#8394,0.900000000000001);
#1254=VECTOR('',#8401,0.900000000000001);
#1255=VECTOR('',#8408,0.900000000000001);
#1256=VECTOR('',#8415,1.35);
#1257=VECTOR('',#8418,1.35);
#1258=VECTOR('',#8427,11.7);
#1259=VECTOR('',#8434,1000.);
#1260=VECTOR('',#8435,1000.);
#1261=VECTOR('',#8438,1000.);
#1262=VECTOR('',#8441,1000.);
#1263=VECTOR('',#8442,1000.);
#1264=VECTOR('',#8443,1000.);
#1265=VECTOR('',#8444,1000.);
#1266=VECTOR('',#8451,1000.);
#1267=VECTOR('',#8454,1000.);
#1268=VECTOR('',#8461,1000.);
#1269=VECTOR('',#8462,1000.);
#1270=VECTOR('',#8463,1000.);
#1271=VECTOR('',#8470,1000.);
#1272=VECTOR('',#8477,1000.);
#1273=VECTOR('',#8482,1000.);
#1274=VECTOR('',#8483,1000.);
#1275=VECTOR('',#8484,1000.);
#1276=VECTOR('',#8487,1000.);
#1277=VECTOR('',#8490,1000.);
#1278=VECTOR('',#8491,1000.);
#1279=VECTOR('',#8492,1000.);
#1280=VECTOR('',#8497,1000.);
#1281=VECTOR('',#8498,1000.);
#1282=VECTOR('',#8501,1000.);
#1283=VECTOR('',#8506,1000.);
#1284=VECTOR('',#8509,1000.);
#1285=VECTOR('',#8510,1000.);
#1286=VECTOR('',#8511,1000.);
#1287=VECTOR('',#8512,1000.);
#1288=VECTOR('',#8513,1000.);
#1289=VECTOR('',#8516,1000.);
#1290=VECTOR('',#8517,1000.);
#1291=VECTOR('',#8518,1000.);
#1292=VECTOR('',#8519,1000.);
#1293=VECTOR('',#8520,1000.);
#1294=VECTOR('',#8523,1000.);
#1295=VECTOR('',#8524,1000.);
#1296=VECTOR('',#8525,1000.);
#1297=VECTOR('',#8528,1000.);
#1298=VECTOR('',#8529,1000.);
#1299=VECTOR('',#8530,1000.);
#1300=VECTOR('',#8531,1000.);
#1301=VECTOR('',#8570,1000.);
#1302=VECTOR('',#8571,1000.);
#1303=VECTOR('',#8572,1000.);
#1304=VECTOR('',#8573,1000.);
#1305=VECTOR('',#8576,1000.);
#1306=VECTOR('',#8581,1000.);
#1307=VECTOR('',#8584,1000.);
#1308=VECTOR('',#8585,1000.);
#1309=VECTOR('',#8590,1000.);
#1310=VECTOR('',#8595,1000.);
#1311=VECTOR('',#8602,1000.);
#1312=VECTOR('',#8605,1000.);
#1313=VECTOR('',#8618,1.2);
#1314=VECTOR('',#8625,0.800000000000001);
#1315=VECTOR('',#8632,0.800000000000001);
#1316=VECTOR('',#8639,0.800000000000001);
#1317=VECTOR('',#8646,1.2);
#1318=VECTOR('',#8649,1.2);
#1319=VECTOR('',#8658,10.4);
#1320=VECTOR('',#8663,1000.);
#1321=VECTOR('',#8666,1000.);
#1322=VECTOR('',#8671,1000.);
#1323=VECTOR('',#8672,1000.);
#1324=VECTOR('',#8681,1000.);
#1325=VECTOR('',#8682,1000.);
#1326=VECTOR('',#8685,1000.);
#1327=VECTOR('',#8688,1000.);
#1328=VECTOR('',#8689,1000.);
#1329=VECTOR('',#8690,1000.);
#1330=VECTOR('',#8691,1000.);
#1331=VECTOR('',#8698,1000.);
#1332=VECTOR('',#8701,1000.);
#1333=VECTOR('',#8706,1000.);
#1334=VECTOR('',#8707,1000.);
#1335=VECTOR('',#8708,1000.);
#1336=VECTOR('',#8717,1000.);
#1337=VECTOR('',#8724,1000.);
#1338=VECTOR('',#8731,1000.);
#1339=VECTOR('',#8732,1000.);
#1340=VECTOR('',#8733,1000.);
#1341=VECTOR('',#8736,1000.);
#1342=VECTOR('',#8739,1000.);
#1343=VECTOR('',#8740,1000.);
#1344=VECTOR('',#8741,1000.);
#1345=VECTOR('',#8746,1000.);
#1346=VECTOR('',#8747,1000.);
#1347=VECTOR('',#8750,1000.);
#1348=VECTOR('',#8755,1000.);
#1349=VECTOR('',#8758,1000.);
#1350=VECTOR('',#8759,1000.);
#1351=VECTOR('',#8760,1000.);
#1352=VECTOR('',#8761,1000.);
#1353=VECTOR('',#8762,1000.);
#1354=VECTOR('',#8765,1000.);
#1355=VECTOR('',#8766,1000.);
#1356=VECTOR('',#8767,1000.);
#1357=VECTOR('',#8768,1000.);
#1358=VECTOR('',#8769,1000.);
#1359=VECTOR('',#8772,1000.);
#1360=VECTOR('',#8773,1000.);
#1361=VECTOR('',#8774,1000.);
#1362=VECTOR('',#8777,1000.);
#1363=VECTOR('',#8778,1000.);
#1364=VECTOR('',#8779,1000.);
#1365=VECTOR('',#8780,1000.);
#1366=VECTOR('',#8819,1000.);
#1367=VECTOR('',#8820,1000.);
#1368=VECTOR('',#8821,1000.);
#1369=VECTOR('',#8822,1000.);
#1370=VECTOR('',#8825,1000.);
#1371=VECTOR('',#8830,1000.);
#1372=VECTOR('',#8833,1000.);
#1373=VECTOR('',#8834,1000.);
#1374=VECTOR('',#8839,1000.);
#1375=VECTOR('',#8844,1000.);
#1376=VECTOR('',#8857,1000.);
#1377=VECTOR('',#8860,1000.);
#1378=VECTOR('',#8873,1.825);
#1379=VECTOR('',#8880,1.095);
#1380=VECTOR('',#8887,2.92);
#1381=VECTOR('',#8892,1000.);
#1382=VECTOR('',#8893,1000.);
#1383=VECTOR('',#8894,1000.);
#1384=VECTOR('',#8895,1000.);
#1385=VECTOR('',#8902,1000.);
#1386=VECTOR('',#8903,1000.);
#1387=VECTOR('',#8906,1000.);
#1388=VECTOR('',#8907,1000.);
#1389=VECTOR('',#8910,1000.);
#1390=VECTOR('',#8915,1000.);
#1391=VECTOR('',#8926,0.729999999999999);
#1392=VECTOR('',#8933,1000.);
#1393=VECTOR('',#8936,1000.);
#1394=VECTOR('',#8941,1.825);
#1395=VECTOR('',#8946,1000.);
#1396=VECTOR('',#8947,1000.);
#1397=VECTOR('',#8948,1000.);
#1398=VECTOR('',#8949,1000.);
#1399=VECTOR('',#8954,1000.);
#1400=VECTOR('',#8955,1000.);
#1401=VECTOR('',#8958,1000.);
#1402=VECTOR('',#8961,1000.);
#1403=VECTOR('',#8976,1.825);
#1404=VECTOR('',#8983,1.095);
#1405=VECTOR('',#8990,2.92);
#1406=VECTOR('',#8995,1000.);
#1407=VECTOR('',#8996,1000.);
#1408=VECTOR('',#8997,1000.);
#1409=VECTOR('',#8998,1000.);
#1410=VECTOR('',#9005,1000.);
#1411=VECTOR('',#9006,1000.);
#1412=VECTOR('',#9009,1000.);
#1413=VECTOR('',#9010,1000.);
#1414=VECTOR('',#9013,1000.);
#1415=VECTOR('',#9018,1000.);
#1416=VECTOR('',#9029,0.730000000000001);
#1417=VECTOR('',#9036,1000.);
#1418=VECTOR('',#9039,1000.);
#1419=VECTOR('',#9044,1.825);
#1420=VECTOR('',#9049,1000.);
#1421=VECTOR('',#9050,1000.);
#1422=VECTOR('',#9051,1000.);
#1423=VECTOR('',#9052,1000.);
#1424=VECTOR('',#9057,1000.);
#1425=VECTOR('',#9058,1000.);
#1426=VECTOR('',#9061,1000.);
#1427=VECTOR('',#9064,1000.);
#1428=VECTOR('',#9079,2.5);
#1429=VECTOR('',#9086,1.5);
#1430=VECTOR('',#9093,4.);
#1431=VECTOR('',#9098,1000.);
#1432=VECTOR('',#9099,1000.);
#1433=VECTOR('',#9100,1000.);
#1434=VECTOR('',#9101,1000.);
#1435=VECTOR('',#9108,1000.);
#1436=VECTOR('',#9109,1000.);
#1437=VECTOR('',#9112,1000.);
#1438=VECTOR('',#9113,1000.);
#1439=VECTOR('',#9116,1000.);
#1440=VECTOR('',#9121,1000.);
#1441=VECTOR('',#9132,1.);
#1442=VECTOR('',#9139,1000.);
#1443=VECTOR('',#9142,1000.);
#1444=VECTOR('',#9147,2.50000000000001);
#1445=VECTOR('',#9152,1000.);
#1446=VECTOR('',#9153,1000.);
#1447=VECTOR('',#9154,1000.);
#1448=VECTOR('',#9155,1000.);
#1449=VECTOR('',#9160,1000.);
#1450=VECTOR('',#9161,1000.);
#1451=VECTOR('',#9164,1000.);
#1452=VECTOR('',#9167,1000.);
#1453=VECTOR('',#9176,1.);
#1454=VECTOR('',#9183,1.);
#1455=VECTOR('',#9190,1.);
#1456=VECTOR('',#9195,1000.);
#1457=VECTOR('',#9196,1000.);
#1458=VECTOR('',#9197,1000.);
#1459=VECTOR('',#9198,1000.);
#1460=VECTOR('',#9201,1000.);
#1461=VECTOR('',#9202,1000.);
#1462=VECTOR('',#9203,1000.);
#1463=VECTOR('',#9204,1000.);
#1464=VECTOR('',#9205,1000.);
#1465=VECTOR('',#9208,1000.);
#1466=VECTOR('',#9209,1000.);
#1467=VECTOR('',#9210,1000.);
#1468=VECTOR('',#9213,1000.);
#1469=VECTOR('',#9214,1000.);
#1470=VECTOR('',#9215,1000.);
#1471=VECTOR('',#9216,1000.);
#1472=VECTOR('',#9217,1000.);
#1473=VECTOR('',#9220,1000.);
#1474=VECTOR('',#9221,1000.);
#1475=VECTOR('',#9226,1000.);
#1476=VECTOR('',#9227,1000.);
#1477=VECTOR('',#9228,1000.);
#1478=VECTOR('',#9229,1000.);
#1479=VECTOR('',#9232,1000.);
#1480=VECTOR('',#9233,1000.);
#1481=VECTOR('',#9234,1000.);
#1482=VECTOR('',#9235,1000.);
#1483=VECTOR('',#9238,1000.);
#1484=VECTOR('',#9241,1000.);
#1485=VECTOR('',#9244,1000.);
#1486=VECTOR('',#9263,1.);
#1487=VECTOR('',#9266,1.);
#1488=VECTOR('',#9277,1000.);
#1489=VECTOR('',#9280,1000.);
#1490=VECTOR('',#9283,1000.);
#1491=VECTOR('',#9284,1000.);
#1492=VECTOR('',#9285,1000.);
#1493=VECTOR('',#9286,1000.);
#1494=VECTOR('',#9289,1000.);
#1495=VECTOR('',#9290,1000.);
#1496=VECTOR('',#9293,1000.);
#1497=VECTOR('',#9296,1000.);
#1498=VECTOR('',#9321,1.);
#1499=VECTOR('',#9328,1.5);
#1500=VECTOR('',#9335,1.5);
#1501=VECTOR('',#9342,1.5);
#1502=VECTOR('',#9381,1000.);
#1503=VECTOR('',#9382,1000.);
#1504=VECTOR('',#9383,1000.);
#1505=VECTOR('',#9384,1000.);
#1506=VECTOR('',#9387,1000.);
#1507=VECTOR('',#9388,1000.);
#1508=VECTOR('',#9389,1000.);
#1509=VECTOR('',#9392,1000.);
#1510=VECTOR('',#9393,1000.);
#1511=VECTOR('',#9396,1000.);
#1512=VECTOR('',#9397,1000.);
#1513=VECTOR('',#9400,1000.);
#1514=VECTOR('',#9405,1000.);
#1515=VECTOR('',#9406,1000.);
#1516=VECTOR('',#9409,1000.);
#1517=VECTOR('',#9410,1000.);
#1518=VECTOR('',#9413,1000.);
#1519=VECTOR('',#9418,1000.);
#1520=VECTOR('',#9419,1000.);
#1521=VECTOR('',#9420,1000.);
#1522=VECTOR('',#9421,1000.);
#1523=VECTOR('',#9422,1000.);
#1524=VECTOR('',#9423,1000.);
#1525=VECTOR('',#9426,1000.);
#1526=VECTOR('',#9427,1000.);
#1527=VECTOR('',#9430,1000.);
#1528=VECTOR('',#9431,1000.);
#1529=VECTOR('',#9432,1000.);
#1530=VECTOR('',#9433,1000.);
#1531=VECTOR('',#9434,1000.);
#1532=VECTOR('',#9439,1000.);
#1533=VECTOR('',#9442,1000.);
#1534=VECTOR('',#9443,1000.);
#1535=VECTOR('',#9454,1.5);
#1536=VECTOR('',#9461,1.65);
#1537=VECTOR('',#9464,1.65);
#1538=VECTOR('',#9469,1000.);
#1539=VECTOR('',#9470,1000.);
#1540=VECTOR('',#9471,1000.);
#1541=VECTOR('',#9476,1000.);
#1542=VECTOR('',#9479,1000.);
#1543=VECTOR('',#9480,1000.);
#1544=VECTOR('',#9487,1000.);
#1545=VECTOR('',#9490,1000.);
#1546=VECTOR('',#9501,1000.);
#1547=VECTOR('',#9504,1000.);
#1548=VECTOR('',#9507,1000.);
#1549=VECTOR('',#9514,1000.);
#1550=VECTOR('',#9515,1000.);
#1551=VECTOR('',#9518,1000.);
#1552=VECTOR('',#9519,1000.);
#1553=VECTOR('',#9522,1000.);
#1554=VECTOR('',#9527,1000.);
#1555=VECTOR('',#9528,1000.);
#1556=VECTOR('',#9529,1000.);
#1557=VECTOR('',#9532,1000.);
#1558=VECTOR('',#9533,1000.);
#1559=VECTOR('',#9534,1000.);
#1560=VECTOR('',#9537,1000.);
#1561=VECTOR('',#9538,1000.);
#1562=VECTOR('',#9549,1.5);
#1563=VECTOR('',#9552,1.5);
#1564=VECTOR('',#9559,1000.);
#1565=VECTOR('',#9562,1000.);
#1566=VECTOR('',#9565,1000.);
#1567=VECTOR('',#9568,1000.);
#1568=VECTOR('',#9575,1.1);
#1569=VECTOR('',#9582,1.1);
#1570=VECTOR('',#9589,1.1);
#1571=VECTOR('',#9600,1000.);
#1572=VECTOR('',#9601,1000.);
#1573=VECTOR('',#9604,1000.);
#1574=VECTOR('',#9609,1000.);
#1575=VECTOR('',#9610,1000.);
#1576=VECTOR('',#9615,1000.);
#1577=VECTOR('',#9616,1000.);
#1578=VECTOR('',#9617,1000.);
#1579=VECTOR('',#9618,1000.);
#1580=VECTOR('',#9627,1000.);
#1581=VECTOR('',#9630,1000.);
#1582=VECTOR('',#9633,1000.);
#1583=VECTOR('',#9636,1000.);
#1584=VECTOR('',#9637,1000.);
#1585=VECTOR('',#9646,1000.);
#1586=VECTOR('',#9647,1000.);
#1587=VECTOR('',#9648,1000.);
#1588=VECTOR('',#9655,1000.);
#1589=VECTOR('',#9656,1000.);
#1590=VECTOR('',#9657,1000.);
#1591=VECTOR('',#9660,1000.);
#1592=VECTOR('',#9665,1000.);
#1593=VECTOR('',#9666,1000.);
#1594=VECTOR('',#9667,1000.);
#1595=VECTOR('',#9670,1000.);
#1596=VECTOR('',#9673,1000.);
#1597=VECTOR('',#9674,1000.);
#1598=VECTOR('',#9675,1000.);
#1599=VECTOR('',#9680,1000.);
#1600=VECTOR('',#9681,1000.);
#1601=VECTOR('',#9684,1000.);
#1602=VECTOR('',#9689,1000.);
#1603=VECTOR('',#9690,10.);
#1604=VECTOR('',#9695,1000.);
#1605=VECTOR('',#9696,1000.);
#1606=VECTOR('',#9697,1000.);
#1607=VECTOR('',#9698,1000.);
#1608=VECTOR('',#9699,1000.);
#1609=VECTOR('',#9702,1000.);
#1610=VECTOR('',#9703,1000.);
#1611=VECTOR('',#9704,1000.);
#1612=VECTOR('',#9705,1000.);
#1613=VECTOR('',#9708,1000.);
#1614=VECTOR('',#9709,1000.);
#1615=VECTOR('',#9710,1000.);
#1616=VECTOR('',#9713,1000.);
#1617=VECTOR('',#9742,1000.);
#1618=VECTOR('',#9743,1000.);
#1619=VECTOR('',#9744,1000.);
#1620=VECTOR('',#9747,1000.);
#1621=VECTOR('',#9774,2.);
#1622=VECTOR('',#9781,1.2);
#1623=VECTOR('',#9788,3.2);
#1624=VECTOR('',#9793,1000.);
#1625=VECTOR('',#9794,1000.);
#1626=VECTOR('',#9795,1000.);
#1627=VECTOR('',#9796,1000.);
#1628=VECTOR('',#9803,1000.);
#1629=VECTOR('',#9804,1000.);
#1630=VECTOR('',#9807,1000.);
#1631=VECTOR('',#9808,1000.);
#1632=VECTOR('',#9811,1000.);
#1633=VECTOR('',#9816,1000.);
#1634=VECTOR('',#9827,0.799999999999998);
#1635=VECTOR('',#9834,1000.);
#1636=VECTOR('',#9837,1000.);
#1637=VECTOR('',#9842,2.);
#1638=VECTOR('',#9847,1000.);
#1639=VECTOR('',#9848,1000.);
#1640=VECTOR('',#9849,1000.);
#1641=VECTOR('',#9850,1000.);
#1642=VECTOR('',#9855,1000.);
#1643=VECTOR('',#9856,1000.);
#1644=VECTOR('',#9859,1000.);
#1645=VECTOR('',#9862,1000.);
#1646=CYLINDRICAL_SURFACE('',#7076,1.5);
#1647=CYLINDRICAL_SURFACE('',#7079,1.5);
#1648=CYLINDRICAL_SURFACE('',#7082,56.4897440054506);
#1649=CYLINDRICAL_SURFACE('',#7099,163.25688730188);
#1650=CYLINDRICAL_SURFACE('',#7105,20.);
#1651=CYLINDRICAL_SURFACE('',#7124,8.);
#1652=CYLINDRICAL_SURFACE('',#7127,2.);
#1653=CYLINDRICAL_SURFACE('',#7136,2.);
#1654=CYLINDRICAL_SURFACE('',#7138,2.);
#1655=CYLINDRICAL_SURFACE('',#7140,2.);
#1656=CYLINDRICAL_SURFACE('',#7141,2.);
#1657=CYLINDRICAL_SURFACE('',#7143,2.);
#1658=CYLINDRICAL_SURFACE('',#7153,2.);
#1659=CYLINDRICAL_SURFACE('',#7155,2.);
#1660=CYLINDRICAL_SURFACE('',#7157,2.);
#1661=CYLINDRICAL_SURFACE('',#7163,2.);
#1662=CYLINDRICAL_SURFACE('',#7165,2.);
#1663=CYLINDRICAL_SURFACE('',#7175,2.);
#1664=CYLINDRICAL_SURFACE('',#7177,2.);
#1665=CYLINDRICAL_SURFACE('',#7179,2.);
#1666=CYLINDRICAL_SURFACE('',#7187,4.54881469766181);
#1667=CYLINDRICAL_SURFACE('',#7190,25.);
#1668=CYLINDRICAL_SURFACE('',#7191,25.);
#1669=CYLINDRICAL_SURFACE('',#7194,2.58323636594183);
#1670=CYLINDRICAL_SURFACE('',#7200,1.5);
#1671=CYLINDRICAL_SURFACE('',#7203,1.);
#1672=CYLINDRICAL_SURFACE('',#7206,1.);
#1673=CYLINDRICAL_SURFACE('',#7209,1.);
#1674=CYLINDRICAL_SURFACE('',#7212,1.5);
#1675=CYLINDRICAL_SURFACE('',#7214,1.5);
#1676=CYLINDRICAL_SURFACE('',#7228,35.);
#1677=CYLINDRICAL_SURFACE('',#7231,26.);
#1678=CYLINDRICAL_SURFACE('',#7258,1.);
#1679=CYLINDRICAL_SURFACE('',#7259,1.);
#1680=CYLINDRICAL_SURFACE('',#7260,1.);
#1681=CYLINDRICAL_SURFACE('',#7261,1.);
#1682=CYLINDRICAL_SURFACE('',#7262,1.);
#1683=CYLINDRICAL_SURFACE('',#7272,3.);
#1684=CYLINDRICAL_SURFACE('',#7273,3.);
#1685=CYLINDRICAL_SURFACE('',#7275,1.35);
#1686=CYLINDRICAL_SURFACE('',#7278,0.900000000000001);
#1687=CYLINDRICAL_SURFACE('',#7281,0.900000000000001);
#1688=CYLINDRICAL_SURFACE('',#7284,0.900000000000001);
#1689=CYLINDRICAL_SURFACE('',#7287,1.35);
#1690=CYLINDRICAL_SURFACE('',#7289,1.35);
#1691=CYLINDRICAL_SURFACE('',#7295,31.5);
#1692=CYLINDRICAL_SURFACE('',#7301,23.4);
#1693=CYLINDRICAL_SURFACE('',#7337,0.9);
#1694=CYLINDRICAL_SURFACE('',#7338,0.9);
#1695=CYLINDRICAL_SURFACE('',#7339,0.9);
#1696=CYLINDRICAL_SURFACE('',#7340,0.9);
#1697=CYLINDRICAL_SURFACE('',#7341,0.9);
#1698=CYLINDRICAL_SURFACE('',#7342,0.9);
#1699=CYLINDRICAL_SURFACE('',#7352,2.7);
#1700=CYLINDRICAL_SURFACE('',#7353,2.7);
#1701=CYLINDRICAL_SURFACE('',#7354,15.4750964764976);
#1702=CYLINDRICAL_SURFACE('',#7355,15.4750964764976);
#1703=CYLINDRICAL_SURFACE('',#7356,10.);
#1704=CYLINDRICAL_SURFACE('',#7357,10.);
#1705=CYLINDRICAL_SURFACE('',#7360,1.2);
#1706=CYLINDRICAL_SURFACE('',#7363,0.800000000000001);
#1707=CYLINDRICAL_SURFACE('',#7366,0.800000000000001);
#1708=CYLINDRICAL_SURFACE('',#7369,0.800000000000001);
#1709=CYLINDRICAL_SURFACE('',#7372,1.2);
#1710=CYLINDRICAL_SURFACE('',#7374,1.2);
#1711=CYLINDRICAL_SURFACE('',#7380,16.7532667406203);
#1712=CYLINDRICAL_SURFACE('',#7382,16.7532667406203);
#1713=CYLINDRICAL_SURFACE('',#7386,28.);
#1714=CYLINDRICAL_SURFACE('',#7392,20.8);
#1715=CYLINDRICAL_SURFACE('',#7429,0.8);
#1716=CYLINDRICAL_SURFACE('',#7430,0.8);
#1717=CYLINDRICAL_SURFACE('',#7431,0.8);
#1718=CYLINDRICAL_SURFACE('',#7432,0.8);
#1719=CYLINDRICAL_SURFACE('',#7433,0.8);
#1720=CYLINDRICAL_SURFACE('',#7434,0.8);
#1721=CYLINDRICAL_SURFACE('',#7444,2.4);
#1722=CYLINDRICAL_SURFACE('',#7445,2.4);
#1723=CYLINDRICAL_SURFACE('',#7446,10.);
#1724=CYLINDRICAL_SURFACE('',#7447,10.);
#1725=CYLINDRICAL_SURFACE('',#7448,4.06015460582196);
#1726=CYLINDRICAL_SURFACE('',#7449,4.06015460582196);
#1727=CYLINDRICAL_SURFACE('',#7450,4.06015460582196);
#1728=CYLINDRICAL_SURFACE('',#7451,22.);
#1729=CYLINDRICAL_SURFACE('',#7452,22.);
#1730=CYLINDRICAL_SURFACE('',#7455,1.825);
#1731=CYLINDRICAL_SURFACE('',#7458,1.095);
#1732=CYLINDRICAL_SURFACE('',#7461,2.92);
#1733=CYLINDRICAL_SURFACE('',#7472,2.19);
#1734=CYLINDRICAL_SURFACE('',#7475,0.729999999999999);
#1735=CYLINDRICAL_SURFACE('',#7478,1.46);
#1736=CYLINDRICAL_SURFACE('',#7481,1.825);
#1737=CYLINDRICAL_SURFACE('',#7494,1.825);
#1738=CYLINDRICAL_SURFACE('',#7497,1.095);
#1739=CYLINDRICAL_SURFACE('',#7500,2.92);
#1740=CYLINDRICAL_SURFACE('',#7511,2.19);
#1741=CYLINDRICAL_SURFACE('',#7514,0.730000000000001);
#1742=CYLINDRICAL_SURFACE('',#7517,1.46);
#1743=CYLINDRICAL_SURFACE('',#7520,1.825);
#1744=CYLINDRICAL_SURFACE('',#7533,2.5);
#1745=CYLINDRICAL_SURFACE('',#7536,1.5);
#1746=CYLINDRICAL_SURFACE('',#7539,4.);
#1747=CYLINDRICAL_SURFACE('',#7550,3.);
#1748=CYLINDRICAL_SURFACE('',#7553,1.);
#1749=CYLINDRICAL_SURFACE('',#7556,2.);
#1750=CYLINDRICAL_SURFACE('',#7559,2.50000000000001);
#1751=CYLINDRICAL_SURFACE('',#7569,1.);
#1752=CYLINDRICAL_SURFACE('',#7572,1.);
#1753=CYLINDRICAL_SURFACE('',#7575,1.);
#1754=CYLINDRICAL_SURFACE('',#7596,1.);
#1755=CYLINDRICAL_SURFACE('',#7598,1.);
#1756=CYLINDRICAL_SURFACE('',#7602,20.);
#1757=CYLINDRICAL_SURFACE('',#7619,1.);
#1758=CYLINDRICAL_SURFACE('',#7622,1.5);
#1759=CYLINDRICAL_SURFACE('',#7625,1.5);
#1760=CYLINDRICAL_SURFACE('',#7628,1.5);
#1761=CYLINDRICAL_SURFACE('',#7667,1.5);
#1762=CYLINDRICAL_SURFACE('',#7670,1.65);
#1763=CYLINDRICAL_SURFACE('',#7672,1.65);
#1764=CYLINDRICAL_SURFACE('',#7676,21.9689920245294);
#1765=CYLINDRICAL_SURFACE('',#7679,21.9689920245294);
#1766=CYLINDRICAL_SURFACE('',#7688,19.25);
#1767=CYLINDRICAL_SURFACE('',#7701,1.5);
#1768=CYLINDRICAL_SURFACE('',#7703,1.5);
#1769=CYLINDRICAL_SURFACE('',#7705,2.84156000253601);
#1770=CYLINDRICAL_SURFACE('',#7711,1.1);
#1771=CYLINDRICAL_SURFACE('',#7714,1.1);
#1772=CYLINDRICAL_SURFACE('',#7717,1.1);
#1773=CYLINDRICAL_SURFACE('',#7731,19.25);
#1774=CYLINDRICAL_SURFACE('',#7766,1.1);
#1775=CYLINDRICAL_SURFACE('',#7767,1.1);
#1776=CYLINDRICAL_SURFACE('',#7768,1.1);
#1777=CYLINDRICAL_SURFACE('',#7769,1.1);
#1778=CYLINDRICAL_SURFACE('',#7770,1.1);
#1779=CYLINDRICAL_SURFACE('',#7771,35.0622035609646);
#1780=CYLINDRICAL_SURFACE('',#7774,10.);
#1781=CYLINDRICAL_SURFACE('',#7775,10.);
#1782=CYLINDRICAL_SURFACE('',#7784,2.);
#1783=CYLINDRICAL_SURFACE('',#7787,1.2);
#1784=CYLINDRICAL_SURFACE('',#7790,3.2);
#1785=CYLINDRICAL_SURFACE('',#7801,2.4);
#1786=CYLINDRICAL_SURFACE('',#7804,0.799999999999998);
#1787=CYLINDRICAL_SURFACE('',#7807,1.6);
#1788=CYLINDRICAL_SURFACE('',#7810,2.);
#1789=SPHERICAL_SURFACE('',#7072,2.);
#1790=SPHERICAL_SURFACE('',#7130,2.);
#1791=SPHERICAL_SURFACE('',#7133,2.);
#1792=SPHERICAL_SURFACE('',#7146,2.);
#1793=SPHERICAL_SURFACE('',#7148,2.);
#1794=SPHERICAL_SURFACE('',#7151,2.);
#1795=SPHERICAL_SURFACE('',#7167,2.);
#1796=SPHERICAL_SURFACE('',#7171,2.);
#1797=SPHERICAL_SURFACE('',#7173,2.);
#1798=SPHERICAL_SURFACE('',#7184,2.);
#1799=SPHERICAL_SURFACE('',#7631,17.5);
#1800=FACE_OUTER_BOUND('',#2191,.T.);
#1801=FACE_OUTER_BOUND('',#2192,.T.);
#1802=FACE_OUTER_BOUND('',#2193,.T.);
#1803=FACE_OUTER_BOUND('',#2194,.T.);
#1804=FACE_OUTER_BOUND('',#2195,.T.);
#1805=FACE_OUTER_BOUND('',#2196,.T.);
#1806=FACE_OUTER_BOUND('',#2197,.T.);
#1807=FACE_OUTER_BOUND('',#2198,.T.);
#1808=FACE_OUTER_BOUND('',#2200,.T.);
#1809=FACE_OUTER_BOUND('',#2201,.T.);
#1810=FACE_OUTER_BOUND('',#2203,.T.);
#1811=FACE_OUTER_BOUND('',#2205,.T.);
#1812=FACE_OUTER_BOUND('',#2206,.T.);
#1813=FACE_OUTER_BOUND('',#2208,.T.);
#1814=FACE_OUTER_BOUND('',#2209,.T.);
#1815=FACE_OUTER_BOUND('',#2210,.T.);
#1816=FACE_OUTER_BOUND('',#2211,.T.);
#1817=FACE_OUTER_BOUND('',#2212,.T.);
#1818=FACE_OUTER_BOUND('',#2213,.T.);
#1819=FACE_OUTER_BOUND('',#2214,.T.);
#1820=FACE_OUTER_BOUND('',#2216,.T.);
#1821=FACE_OUTER_BOUND('',#2218,.T.);
#1822=FACE_OUTER_BOUND('',#2219,.T.);
#1823=FACE_OUTER_BOUND('',#2220,.T.);
#1824=FACE_OUTER_BOUND('',#2221,.T.);
#1825=FACE_OUTER_BOUND('',#2222,.T.);
#1826=FACE_OUTER_BOUND('',#2223,.T.);
#1827=FACE_OUTER_BOUND('',#2224,.T.);
#1828=FACE_OUTER_BOUND('',#2225,.T.);
#1829=FACE_OUTER_BOUND('',#2226,.T.);
#1830=FACE_OUTER_BOUND('',#2227,.T.);
#1831=FACE_OUTER_BOUND('',#2228,.T.);
#1832=FACE_OUTER_BOUND('',#2229,.T.);
#1833=FACE_OUTER_BOUND('',#2230,.T.);
#1834=FACE_OUTER_BOUND('',#2231,.T.);
#1835=FACE_OUTER_BOUND('',#2232,.T.);
#1836=FACE_OUTER_BOUND('',#2233,.T.);
#1837=FACE_OUTER_BOUND('',#2234,.T.);
#1838=FACE_OUTER_BOUND('',#2235,.T.);
#1839=FACE_OUTER_BOUND('',#2236,.T.);
#1840=FACE_OUTER_BOUND('',#2237,.T.);
#1841=FACE_OUTER_BOUND('',#2238,.T.);
#1842=FACE_OUTER_BOUND('',#2239,.T.);
#1843=FACE_OUTER_BOUND('',#2240,.T.);
#1844=FACE_OUTER_BOUND('',#2241,.T.);
#1845=FACE_OUTER_BOUND('',#2242,.T.);
#1846=FACE_OUTER_BOUND('',#2243,.T.);
#1847=FACE_OUTER_BOUND('',#2244,.T.);
#1848=FACE_OUTER_BOUND('',#2245,.T.);
#1849=FACE_OUTER_BOUND('',#2246,.T.);
#1850=FACE_OUTER_BOUND('',#2247,.T.);
#1851=FACE_OUTER_BOUND('',#2248,.T.);
#1852=FACE_OUTER_BOUND('',#2249,.T.);
#1853=FACE_OUTER_BOUND('',#2250,.T.);
#1854=FACE_OUTER_BOUND('',#2251,.T.);
#1855=FACE_OUTER_BOUND('',#2252,.T.);
#1856=FACE_OUTER_BOUND('',#2253,.T.);
#1857=FACE_OUTER_BOUND('',#2254,.T.);
#1858=FACE_OUTER_BOUND('',#2255,.T.);
#1859=FACE_OUTER_BOUND('',#2256,.T.);
#1860=FACE_OUTER_BOUND('',#2257,.T.);
#1861=FACE_OUTER_BOUND('',#2258,.T.);
#1862=FACE_OUTER_BOUND('',#2259,.T.);
#1863=FACE_OUTER_BOUND('',#2260,.T.);
#1864=FACE_OUTER_BOUND('',#2261,.T.);
#1865=FACE_OUTER_BOUND('',#2262,.T.);
#1866=FACE_OUTER_BOUND('',#2263,.T.);
#1867=FACE_OUTER_BOUND('',#2264,.T.);
#1868=FACE_OUTER_BOUND('',#2267,.T.);
#1869=FACE_OUTER_BOUND('',#2268,.T.);
#1870=FACE_OUTER_BOUND('',#2269,.T.);
#1871=FACE_OUTER_BOUND('',#2270,.T.);
#1872=FACE_OUTER_BOUND('',#2271,.T.);
#1873=FACE_OUTER_BOUND('',#2272,.T.);
#1874=FACE_OUTER_BOUND('',#2273,.T.);
#1875=FACE_OUTER_BOUND('',#2275,.T.);
#1876=FACE_OUTER_BOUND('',#2276,.T.);
#1877=FACE_OUTER_BOUND('',#2278,.T.);
#1878=FACE_OUTER_BOUND('',#2280,.T.);
#1879=FACE_OUTER_BOUND('',#2281,.T.);
#1880=FACE_OUTER_BOUND('',#2282,.T.);
#1881=FACE_OUTER_BOUND('',#2284,.T.);
#1882=FACE_OUTER_BOUND('',#2285,.T.);
#1883=FACE_OUTER_BOUND('',#2287,.T.);
#1884=FACE_OUTER_BOUND('',#2288,.T.);
#1885=FACE_OUTER_BOUND('',#2289,.T.);
#1886=FACE_OUTER_BOUND('',#2290,.T.);
#1887=FACE_OUTER_BOUND('',#2291,.T.);
#1888=FACE_OUTER_BOUND('',#2293,.T.);
#1889=FACE_OUTER_BOUND('',#2295,.T.);
#1890=FACE_OUTER_BOUND('',#2296,.T.);
#1891=FACE_OUTER_BOUND('',#2297,.T.);
#1892=FACE_OUTER_BOUND('',#2298,.T.);
#1893=FACE_OUTER_BOUND('',#2299,.T.);
#1894=FACE_OUTER_BOUND('',#2300,.T.);
#1895=FACE_OUTER_BOUND('',#2301,.T.);
#1896=FACE_OUTER_BOUND('',#2302,.T.);
#1897=FACE_OUTER_BOUND('',#2303,.T.);
#1898=FACE_OUTER_BOUND('',#2305,.T.);
#1899=FACE_OUTER_BOUND('',#2306,.T.);
#1900=FACE_OUTER_BOUND('',#2308,.T.);
#1901=FACE_OUTER_BOUND('',#2309,.T.);
#1902=FACE_OUTER_BOUND('',#2310,.T.);
#1903=FACE_OUTER_BOUND('',#2311,.T.);
#1904=FACE_OUTER_BOUND('',#2312,.T.);
#1905=FACE_OUTER_BOUND('',#2313,.T.);
#1906=FACE_OUTER_BOUND('',#2314,.T.);
#1907=FACE_OUTER_BOUND('',#2315,.T.);
#1908=FACE_OUTER_BOUND('',#2316,.T.);
#1909=FACE_OUTER_BOUND('',#2317,.T.);
#1910=FACE_OUTER_BOUND('',#2320,.T.);
#1911=FACE_OUTER_BOUND('',#2321,.T.);
#1912=FACE_OUTER_BOUND('',#2322,.T.);
#1913=FACE_OUTER_BOUND('',#2323,.T.);
#1914=FACE_OUTER_BOUND('',#2325,.T.);
#1915=FACE_OUTER_BOUND('',#2326,.T.);
#1916=FACE_OUTER_BOUND('',#2328,.T.);
#1917=FACE_OUTER_BOUND('',#2330,.T.);
#1918=FACE_OUTER_BOUND('',#2331,.T.);
#1919=FACE_OUTER_BOUND('',#2332,.T.);
#1920=FACE_OUTER_BOUND('',#2334,.T.);
#1921=FACE_OUTER_BOUND('',#2335,.T.);
#1922=FACE_OUTER_BOUND('',#2337,.T.);
#1923=FACE_OUTER_BOUND('',#2338,.T.);
#1924=FACE_OUTER_BOUND('',#2339,.T.);
#1925=FACE_OUTER_BOUND('',#2340,.T.);
#1926=FACE_OUTER_BOUND('',#2341,.T.);
#1927=FACE_OUTER_BOUND('',#2343,.T.);
#1928=FACE_OUTER_BOUND('',#2345,.T.);
#1929=FACE_OUTER_BOUND('',#2346,.T.);
#1930=FACE_OUTER_BOUND('',#2347,.T.);
#1931=FACE_OUTER_BOUND('',#2348,.T.);
#1932=FACE_OUTER_BOUND('',#2349,.T.);
#1933=FACE_OUTER_BOUND('',#2350,.T.);
#1934=FACE_OUTER_BOUND('',#2351,.T.);
#1935=FACE_OUTER_BOUND('',#2352,.T.);
#1936=FACE_OUTER_BOUND('',#2353,.T.);
#1937=FACE_OUTER_BOUND('',#2354,.T.);
#1938=FACE_OUTER_BOUND('',#2356,.T.);
#1939=FACE_OUTER_BOUND('',#2357,.T.);
#1940=FACE_OUTER_BOUND('',#2359,.T.);
#1941=FACE_OUTER_BOUND('',#2360,.T.);
#1942=FACE_OUTER_BOUND('',#2361,.T.);
#1943=FACE_OUTER_BOUND('',#2362,.T.);
#1944=FACE_OUTER_BOUND('',#2363,.T.);
#1945=FACE_OUTER_BOUND('',#2364,.T.);
#1946=FACE_OUTER_BOUND('',#2365,.T.);
#1947=FACE_OUTER_BOUND('',#2366,.T.);
#1948=FACE_OUTER_BOUND('',#2367,.T.);
#1949=FACE_OUTER_BOUND('',#2368,.T.);
#1950=FACE_OUTER_BOUND('',#2369,.T.);
#1951=FACE_OUTER_BOUND('',#2370,.T.);
#1952=FACE_OUTER_BOUND('',#2371,.T.);
#1953=FACE_OUTER_BOUND('',#2372,.T.);
#1954=FACE_OUTER_BOUND('',#2373,.T.);
#1955=FACE_OUTER_BOUND('',#2376,.T.);
#1956=FACE_OUTER_BOUND('',#2377,.T.);
#1957=FACE_OUTER_BOUND('',#2378,.T.);
#1958=FACE_OUTER_BOUND('',#2380,.T.);
#1959=FACE_OUTER_BOUND('',#2381,.T.);
#1960=FACE_OUTER_BOUND('',#2382,.T.);
#1961=FACE_OUTER_BOUND('',#2383,.T.);
#1962=FACE_OUTER_BOUND('',#2385,.T.);
#1963=FACE_OUTER_BOUND('',#2386,.T.);
#1964=FACE_OUTER_BOUND('',#2388,.T.);
#1965=FACE_OUTER_BOUND('',#2390,.T.);
#1966=FACE_OUTER_BOUND('',#2391,.T.);
#1967=FACE_OUTER_BOUND('',#2392,.T.);
#1968=FACE_OUTER_BOUND('',#2394,.T.);
#1969=FACE_OUTER_BOUND('',#2395,.T.);
#1970=FACE_OUTER_BOUND('',#2397,.T.);
#1971=FACE_OUTER_BOUND('',#2398,.T.);
#1972=FACE_OUTER_BOUND('',#2399,.T.);
#1973=FACE_OUTER_BOUND('',#2400,.T.);
#1974=FACE_OUTER_BOUND('',#2401,.T.);
#1975=FACE_OUTER_BOUND('',#2403,.T.);
#1976=FACE_OUTER_BOUND('',#2405,.T.);
#1977=FACE_OUTER_BOUND('',#2406,.T.);
#1978=FACE_OUTER_BOUND('',#2407,.T.);
#1979=FACE_OUTER_BOUND('',#2408,.T.);
#1980=FACE_OUTER_BOUND('',#2409,.T.);
#1981=FACE_OUTER_BOUND('',#2410,.T.);
#1982=FACE_OUTER_BOUND('',#2411,.T.);
#1983=FACE_OUTER_BOUND('',#2412,.T.);
#1984=FACE_OUTER_BOUND('',#2413,.T.);
#1985=FACE_OUTER_BOUND('',#2414,.T.);
#1986=FACE_OUTER_BOUND('',#2416,.T.);
#1987=FACE_OUTER_BOUND('',#2417,.T.);
#1988=FACE_OUTER_BOUND('',#2419,.T.);
#1989=FACE_OUTER_BOUND('',#2420,.T.);
#1990=FACE_OUTER_BOUND('',#2421,.T.);
#1991=FACE_OUTER_BOUND('',#2422,.T.);
#1992=FACE_OUTER_BOUND('',#2423,.T.);
#1993=FACE_OUTER_BOUND('',#2424,.T.);
#1994=FACE_OUTER_BOUND('',#2425,.T.);
#1995=FACE_OUTER_BOUND('',#2426,.T.);
#1996=FACE_OUTER_BOUND('',#2427,.T.);
#1997=FACE_OUTER_BOUND('',#2428,.T.);
#1998=FACE_OUTER_BOUND('',#2429,.T.);
#1999=FACE_OUTER_BOUND('',#2430,.T.);
#2000=FACE_OUTER_BOUND('',#2431,.T.);
#2001=FACE_OUTER_BOUND('',#2432,.T.);
#2002=FACE_OUTER_BOUND('',#2434,.T.);
#2003=FACE_OUTER_BOUND('',#2436,.T.);
#2004=FACE_OUTER_BOUND('',#2438,.T.);
#2005=FACE_OUTER_BOUND('',#2439,.T.);
#2006=FACE_OUTER_BOUND('',#2441,.T.);
#2007=FACE_OUTER_BOUND('',#2442,.T.);
#2008=FACE_OUTER_BOUND('',#2443,.T.);
#2009=FACE_OUTER_BOUND('',#2444,.T.);
#2010=FACE_OUTER_BOUND('',#2445,.T.);
#2011=FACE_OUTER_BOUND('',#2446,.T.);
#2012=FACE_OUTER_BOUND('',#2447,.T.);
#2013=FACE_OUTER_BOUND('',#2449,.T.);
#2014=FACE_OUTER_BOUND('',#2450,.T.);
#2015=FACE_OUTER_BOUND('',#2452,.T.);
#2016=FACE_OUTER_BOUND('',#2453,.T.);
#2017=FACE_OUTER_BOUND('',#2455,.T.);
#2018=FACE_OUTER_BOUND('',#2456,.T.);
#2019=FACE_OUTER_BOUND('',#2457,.T.);
#2020=FACE_OUTER_BOUND('',#2458,.T.);
#2021=FACE_OUTER_BOUND('',#2459,.T.);
#2022=FACE_OUTER_BOUND('',#2461,.T.);
#2023=FACE_OUTER_BOUND('',#2463,.T.);
#2024=FACE_OUTER_BOUND('',#2465,.T.);
#2025=FACE_OUTER_BOUND('',#2466,.T.);
#2026=FACE_OUTER_BOUND('',#2468,.T.);
#2027=FACE_OUTER_BOUND('',#2469,.T.);
#2028=FACE_OUTER_BOUND('',#2470,.T.);
#2029=FACE_OUTER_BOUND('',#2471,.T.);
#2030=FACE_OUTER_BOUND('',#2472,.T.);
#2031=FACE_OUTER_BOUND('',#2473,.T.);
#2032=FACE_OUTER_BOUND('',#2474,.T.);
#2033=FACE_OUTER_BOUND('',#2476,.T.);
#2034=FACE_OUTER_BOUND('',#2477,.T.);
#2035=FACE_OUTER_BOUND('',#2479,.T.);
#2036=FACE_OUTER_BOUND('',#2480,.T.);
#2037=FACE_OUTER_BOUND('',#2482,.T.);
#2038=FACE_OUTER_BOUND('',#2483,.T.);
#2039=FACE_OUTER_BOUND('',#2484,.T.);
#2040=FACE_OUTER_BOUND('',#2485,.T.);
#2041=FACE_OUTER_BOUND('',#2486,.T.);
#2042=FACE_OUTER_BOUND('',#2488,.T.);
#2043=FACE_OUTER_BOUND('',#2490,.T.);
#2044=FACE_OUTER_BOUND('',#2492,.T.);
#2045=FACE_OUTER_BOUND('',#2493,.T.);
#2046=FACE_OUTER_BOUND('',#2495,.T.);
#2047=FACE_OUTER_BOUND('',#2496,.T.);
#2048=FACE_OUTER_BOUND('',#2497,.T.);
#2049=FACE_OUTER_BOUND('',#2498,.T.);
#2050=FACE_OUTER_BOUND('',#2499,.T.);
#2051=FACE_OUTER_BOUND('',#2500,.T.);
#2052=FACE_OUTER_BOUND('',#2501,.T.);
#2053=FACE_OUTER_BOUND('',#2503,.T.);
#2054=FACE_OUTER_BOUND('',#2504,.T.);
#2055=FACE_OUTER_BOUND('',#2506,.T.);
#2056=FACE_OUTER_BOUND('',#2507,.T.);
#2057=FACE_OUTER_BOUND('',#2509,.T.);
#2058=FACE_OUTER_BOUND('',#2510,.T.);
#2059=FACE_OUTER_BOUND('',#2511,.T.);
#2060=FACE_OUTER_BOUND('',#2512,.T.);
#2061=FACE_OUTER_BOUND('',#2513,.T.);
#2062=FACE_OUTER_BOUND('',#2514,.T.);
#2063=FACE_OUTER_BOUND('',#2516,.T.);
#2064=FACE_OUTER_BOUND('',#2517,.T.);
#2065=FACE_OUTER_BOUND('',#2519,.T.);
#2066=FACE_OUTER_BOUND('',#2520,.T.);
#2067=FACE_OUTER_BOUND('',#2521,.T.);
#2068=FACE_OUTER_BOUND('',#2522,.T.);
#2069=FACE_OUTER_BOUND('',#2523,.T.);
#2070=FACE_OUTER_BOUND('',#2524,.T.);
#2071=FACE_OUTER_BOUND('',#2526,.T.);
#2072=FACE_OUTER_BOUND('',#2528,.T.);
#2073=FACE_OUTER_BOUND('',#2529,.T.);
#2074=FACE_OUTER_BOUND('',#2530,.T.);
#2075=FACE_OUTER_BOUND('',#2531,.T.);
#2076=FACE_OUTER_BOUND('',#2532,.T.);
#2077=FACE_OUTER_BOUND('',#2533,.T.);
#2078=FACE_OUTER_BOUND('',#2534,.T.);
#2079=FACE_OUTER_BOUND('',#2537,.T.);
#2080=FACE_OUTER_BOUND('',#2539,.T.);
#2081=FACE_OUTER_BOUND('',#2540,.T.);
#2082=FACE_OUTER_BOUND('',#2541,.T.);
#2083=FACE_OUTER_BOUND('',#2543,.T.);
#2084=FACE_OUTER_BOUND('',#2544,.T.);
#2085=FACE_OUTER_BOUND('',#2546,.T.);
#2086=FACE_OUTER_BOUND('',#2547,.T.);
#2087=FACE_OUTER_BOUND('',#2548,.T.);
#2088=FACE_OUTER_BOUND('',#2549,.T.);
#2089=FACE_OUTER_BOUND('',#2550,.T.);
#2090=FACE_OUTER_BOUND('',#2553,.T.);
#2091=FACE_OUTER_BOUND('',#2554,.T.);
#2092=FACE_OUTER_BOUND('',#2555,.T.);
#2093=FACE_OUTER_BOUND('',#2557,.T.);
#2094=FACE_OUTER_BOUND('',#2558,.T.);
#2095=FACE_OUTER_BOUND('',#2560,.T.);
#2096=FACE_OUTER_BOUND('',#2561,.T.);
#2097=FACE_OUTER_BOUND('',#2563,.T.);
#2098=FACE_OUTER_BOUND('',#2564,.T.);
#2099=FACE_OUTER_BOUND('',#2566,.T.);
#2100=FACE_OUTER_BOUND('',#2567,.T.);
#2101=FACE_OUTER_BOUND('',#2568,.T.);
#2102=FACE_OUTER_BOUND('',#2569,.T.);
#2103=FACE_OUTER_BOUND('',#2570,.T.);
#2104=FACE_OUTER_BOUND('',#2571,.T.);
#2105=FACE_OUTER_BOUND('',#2572,.T.);
#2106=FACE_OUTER_BOUND('',#2573,.T.);
#2107=FACE_OUTER_BOUND('',#2575,.T.);
#2108=FACE_OUTER_BOUND('',#2577,.T.);
#2109=FACE_OUTER_BOUND('',#2578,.T.);
#2110=FACE_OUTER_BOUND('',#2579,.T.);
#2111=FACE_OUTER_BOUND('',#2580,.T.);
#2112=FACE_OUTER_BOUND('',#2581,.T.);
#2113=FACE_OUTER_BOUND('',#2582,.T.);
#2114=FACE_OUTER_BOUND('',#2583,.T.);
#2115=FACE_OUTER_BOUND('',#2586,.T.);
#2116=FACE_OUTER_BOUND('',#2587,.T.);
#2117=FACE_OUTER_BOUND('',#2588,.T.);
#2118=FACE_OUTER_BOUND('',#2589,.T.);
#2119=FACE_OUTER_BOUND('',#2591,.T.);
#2120=FACE_OUTER_BOUND('',#2593,.T.);
#2121=FACE_OUTER_BOUND('',#2594,.T.);
#2122=FACE_OUTER_BOUND('',#2595,.T.);
#2123=FACE_OUTER_BOUND('',#2596,.T.);
#2124=FACE_OUTER_BOUND('',#2597,.T.);
#2125=FACE_OUTER_BOUND('',#2598,.T.);
#2126=FACE_OUTER_BOUND('',#2600,.T.);
#2127=FACE_OUTER_BOUND('',#2602,.T.);
#2128=FACE_OUTER_BOUND('',#2603,.T.);
#2129=FACE_OUTER_BOUND('',#2604,.T.);
#2130=FACE_OUTER_BOUND('',#2605,.T.);
#2131=FACE_OUTER_BOUND('',#2606,.T.);
#2132=FACE_OUTER_BOUND('',#2607,.T.);
#2133=FACE_OUTER_BOUND('',#2608,.T.);
#2134=FACE_OUTER_BOUND('',#2611,.T.);
#2135=FACE_OUTER_BOUND('',#2612,.T.);
#2136=FACE_OUTER_BOUND('',#2613,.T.);
#2137=FACE_OUTER_BOUND('',#2614,.T.);
#2138=FACE_OUTER_BOUND('',#2615,.T.);
#2139=FACE_OUTER_BOUND('',#2616,.T.);
#2140=FACE_OUTER_BOUND('',#2617,.T.);
#2141=FACE_OUTER_BOUND('',#2618,.T.);
#2142=FACE_OUTER_BOUND('',#2619,.T.);
#2143=FACE_OUTER_BOUND('',#2621,.T.);
#2144=FACE_OUTER_BOUND('',#2623,.T.);
#2145=FACE_OUTER_BOUND('',#2624,.T.);
#2146=FACE_OUTER_BOUND('',#2625,.T.);
#2147=FACE_OUTER_BOUND('',#2627,.T.);
#2148=FACE_OUTER_BOUND('',#2628,.T.);
#2149=FACE_OUTER_BOUND('',#2630,.T.);
#2150=FACE_OUTER_BOUND('',#2631,.T.);
#2151=FACE_OUTER_BOUND('',#2632,.T.);
#2152=FACE_OUTER_BOUND('',#2633,.T.);
#2153=FACE_OUTER_BOUND('',#2634,.T.);
#2154=FACE_OUTER_BOUND('',#2635,.T.);
#2155=FACE_OUTER_BOUND('',#2637,.T.);
#2156=FACE_OUTER_BOUND('',#2639,.T.);
#2157=FACE_OUTER_BOUND('',#2640,.T.);
#2158=FACE_OUTER_BOUND('',#2641,.T.);
#2159=FACE_OUTER_BOUND('',#2642,.T.);
#2160=FACE_OUTER_BOUND('',#2643,.T.);
#2161=FACE_OUTER_BOUND('',#2644,.T.);
#2162=FACE_OUTER_BOUND('',#2645,.T.);
#2163=FACE_OUTER_BOUND('',#2646,.T.);
#2164=FACE_OUTER_BOUND('',#2647,.T.);
#2165=FACE_OUTER_BOUND('',#2648,.T.);
#2166=FACE_OUTER_BOUND('',#2649,.T.);
#2167=FACE_OUTER_BOUND('',#2650,.T.);
#2168=FACE_OUTER_BOUND('',#2651,.T.);
#2169=FACE_OUTER_BOUND('',#2652,.T.);
#2170=FACE_OUTER_BOUND('',#2653,.T.);
#2171=FACE_OUTER_BOUND('',#2654,.T.);
#2172=FACE_OUTER_BOUND('',#2655,.T.);
#2173=FACE_OUTER_BOUND('',#2656,.T.);
#2174=FACE_OUTER_BOUND('',#2657,.T.);
#2175=FACE_OUTER_BOUND('',#2659,.T.);
#2176=FACE_OUTER_BOUND('',#2661,.T.);
#2177=FACE_OUTER_BOUND('',#2663,.T.);
#2178=FACE_OUTER_BOUND('',#2664,.T.);
#2179=FACE_OUTER_BOUND('',#2666,.T.);
#2180=FACE_OUTER_BOUND('',#2667,.T.);
#2181=FACE_OUTER_BOUND('',#2668,.T.);
#2182=FACE_OUTER_BOUND('',#2669,.T.);
#2183=FACE_OUTER_BOUND('',#2670,.T.);
#2184=FACE_OUTER_BOUND('',#2671,.T.);
#2185=FACE_OUTER_BOUND('',#2672,.T.);
#2186=FACE_OUTER_BOUND('',#2674,.T.);
#2187=FACE_OUTER_BOUND('',#2675,.T.);
#2188=FACE_OUTER_BOUND('',#2677,.T.);
#2189=FACE_OUTER_BOUND('',#2678,.T.);
#2190=FACE_OUTER_BOUND('',#2680,.T.);
#2191=EDGE_LOOP('',(#4558,#4559,#4560,#4561));
#2192=EDGE_LOOP('',(#4562,#4563,#4564,#4565));
#2193=EDGE_LOOP('',(#4566,#4567,#4568));
#2194=EDGE_LOOP('',(#4569,#4570,#4571,#4572));
#2195=EDGE_LOOP('',(#4573,#4574,#4575,#4576));
#2196=EDGE_LOOP('',(#4577,#4578,#4579,#4580));
#2197=EDGE_LOOP('',(#4581,#4582,#4583,#4584));
#2198=EDGE_LOOP('',(#4585,#4586,#4587,#4588,#4589,#4590,#4591,#4592));
#2199=EDGE_LOOP('',(#4593));
#2200=EDGE_LOOP('',(#4594,#4595,#4596,#4597));
#2201=EDGE_LOOP('',(#4598,#4599,#4600,#4601,#4602,#4603,#4604,#4605));
#2202=EDGE_LOOP('',(#4606));
#2203=EDGE_LOOP('',(#4607,#4608,#4609,#4610));
#2204=EDGE_LOOP('',(#4611,#4612,#4613,#4614));
#2205=EDGE_LOOP('',(#4615,#4616,#4617,#4618));
#2206=EDGE_LOOP('',(#4619,#4620,#4621,#4622));
#2207=EDGE_LOOP('',(#4623,#4624,#4625,#4626));
#2208=EDGE_LOOP('',(#4627,#4628,#4629,#4630));
#2209=EDGE_LOOP('',(#4631,#4632,#4633,#4634));
#2210=EDGE_LOOP('',(#4635,#4636,#4637,#4638));
#2211=EDGE_LOOP('',(#4639,#4640,#4641,#4642));
#2212=EDGE_LOOP('',(#4643,#4644,#4645,#4646,#4647,#4648,#4649,#4650));
#2213=EDGE_LOOP('',(#4651,#4652,#4653,#4654,#4655,#4656,#4657,#4658));
#2214=EDGE_LOOP('',(#4659,#4660,#4661,#4662,#4663,#4664,#4665));
#2215=EDGE_LOOP('',(#4666));
#2216=EDGE_LOOP('',(#4667,#4668,#4669,#4670,#4671,#4672,#4673));
#2217=EDGE_LOOP('',(#4674));
#2218=EDGE_LOOP('',(#4675,#4676,#4677,#4678));
#2219=EDGE_LOOP('',(#4679,#4680,#4681,#4682));
#2220=EDGE_LOOP('',(#4683,#4684,#4685,#4686));
#2221=EDGE_LOOP('',(#4687,#4688,#4689,#4690));
#2222=EDGE_LOOP('',(#4691,#4692,#4693,#4694));
#2223=EDGE_LOOP('',(#4695,#4696,#4697,#4698));
#2224=EDGE_LOOP('',(#4699,#4700,#4701));
#2225=EDGE_LOOP('',(#4702,#4703,#4704));
#2226=EDGE_LOOP('',(#4705,#4706,#4707,#4708));
#2227=EDGE_LOOP('',(#4709,#4710,#4711,#4712));
#2228=EDGE_LOOP('',(#4713,#4714,#4715,#4716));
#2229=EDGE_LOOP('',(#4717,#4718,#4719,#4720));
#2230=EDGE_LOOP('',(#4721,#4722,#4723,#4724));
#2231=EDGE_LOOP('',(#4725,#4726,#4727));
#2232=EDGE_LOOP('',(#4728,#4729,#4730));
#2233=EDGE_LOOP('',(#4731,#4732,#4733));
#2234=EDGE_LOOP('',(#4734,#4735,#4736,#4737));
#2235=EDGE_LOOP('',(#4738,#4739,#4740,#4741));
#2236=EDGE_LOOP('',(#4742,#4743,#4744,#4745));
#2237=EDGE_LOOP('',(#4746,#4747,#4748,#4749));
#2238=EDGE_LOOP('',(#4750,#4751,#4752,#4753));
#2239=EDGE_LOOP('',(#4754,#4755,#4756,#4757));
#2240=EDGE_LOOP('',(#4758,#4759,#4760,#4761));
#2241=EDGE_LOOP('',(#4762,#4763,#4764));
#2242=EDGE_LOOP('',(#4765,#4766,#4767,#4768));
#2243=EDGE_LOOP('',(#4769,#4770,#4771));
#2244=EDGE_LOOP('',(#4772,#4773,#4774));
#2245=EDGE_LOOP('',(#4775,#4776,#4777,#4778));
#2246=EDGE_LOOP('',(#4779,#4780,#4781,#4782));
#2247=EDGE_LOOP('',(#4783,#4784,#4785,#4786));
#2248=EDGE_LOOP('',(#4787,#4788,#4789,#4790));
#2249=EDGE_LOOP('',(#4791,#4792,#4793,#4794));
#2250=EDGE_LOOP('',(#4795,#4796,#4797));
#2251=EDGE_LOOP('',(#4798,#4799,#4800,#4801));
#2252=EDGE_LOOP('',(#4802,#4803,#4804,#4805));
#2253=EDGE_LOOP('',(#4806,#4807,#4808,#4809));
#2254=EDGE_LOOP('',(#4810,#4811,#4812,#4813));
#2255=EDGE_LOOP('',(#4814,#4815,#4816,#4817));
#2256=EDGE_LOOP('',(#4818,#4819,#4820,#4821));
#2257=EDGE_LOOP('',(#4822,#4823,#4824,#4825,#4826,#4827,#4828,#4829,#4830,
#4831));
#2258=EDGE_LOOP('',(#4832,#4833,#4834,#4835));
#2259=EDGE_LOOP('',(#4836,#4837,#4838,#4839));
#2260=EDGE_LOOP('',(#4840,#4841,#4842,#4843));
#2261=EDGE_LOOP('',(#4844,#4845,#4846,#4847));
#2262=EDGE_LOOP('',(#4848,#4849,#4850,#4851,#4852));
#2263=EDGE_LOOP('',(#4853,#4854,#4855,#4856,#4857));
#2264=EDGE_LOOP('',(#4858,#4859,#4860,#4861,#4862,#4863,#4864,#4865,#4866,
#4867,#4868,#4869,#4870));
#2265=EDGE_LOOP('',(#4871,#4872));
#2266=EDGE_LOOP('',(#4873,#4874));
#2267=EDGE_LOOP('',(#4875,#4876,#4877));
#2268=EDGE_LOOP('',(#4878,#4879,#4880,#4881));
#2269=EDGE_LOOP('',(#4882,#4883,#4884,#4885));
#2270=EDGE_LOOP('',(#4886,#4887,#4888,#4889));
#2271=EDGE_LOOP('',(#4890,#4891));
#2272=EDGE_LOOP('',(#4892,#4893,#4894,#4895,#4896,#4897));
#2273=EDGE_LOOP('',(#4898,#4899));
#2274=EDGE_LOOP('',(#4900,#4901,#4902,#4903));
#2275=EDGE_LOOP('',(#4904,#4905,#4906,#4907));
#2276=EDGE_LOOP('',(#4908,#4909,#4910,#4911));
#2277=EDGE_LOOP('',(#4912));
#2278=EDGE_LOOP('',(#4913,#4914,#4915,#4916));
#2279=EDGE_LOOP('',(#4917));
#2280=EDGE_LOOP('',(#4918,#4919,#4920,#4921));
#2281=EDGE_LOOP('',(#4922,#4923,#4924,#4925));
#2282=EDGE_LOOP('',(#4926,#4927,#4928,#4929,#4930,#4931,#4932,#4933));
#2283=EDGE_LOOP('',(#4934));
#2284=EDGE_LOOP('',(#4935,#4936,#4937,#4938,#4939));
#2285=EDGE_LOOP('',(#4940,#4941,#4942,#4943,#4944,#4945,#4946,#4947));
#2286=EDGE_LOOP('',(#4948));
#2287=EDGE_LOOP('',(#4949,#4950,#4951,#4952,#4953,#4954,#4955,#4956,#4957,
#4958,#4959,#4960));
#2288=EDGE_LOOP('',(#4961,#4962,#4963,#4964,#4965,#4966,#4967,#4968));
#2289=EDGE_LOOP('',(#4969,#4970,#4971,#4972));
#2290=EDGE_LOOP('',(#4973,#4974,#4975));
#2291=EDGE_LOOP('',(#4976,#4977,#4978,#4979,#4980,#4981));
#2292=EDGE_LOOP('',(#4982));
#2293=EDGE_LOOP('',(#4983,#4984,#4985,#4986,#4987,#4988));
#2294=EDGE_LOOP('',(#4989));
#2295=EDGE_LOOP('',(#4990));
#2296=EDGE_LOOP('',(#4991));
#2297=EDGE_LOOP('',(#4992,#4993,#4994,#4995));
#2298=EDGE_LOOP('',(#4996,#4997,#4998,#4999));
#2299=EDGE_LOOP('',(#5000,#5001,#5002,#5003));
#2300=EDGE_LOOP('',(#5004,#5005,#5006,#5007));
#2301=EDGE_LOOP('',(#5008,#5009,#5010,#5011,#5012,#5013));
#2302=EDGE_LOOP('',(#5014,#5015,#5016,#5017));
#2303=EDGE_LOOP('',(#5018,#5019,#5020,#5021,#5022,#5023));
#2304=EDGE_LOOP('',(#5024));
#2305=EDGE_LOOP('',(#5025,#5026,#5027,#5028));
#2306=EDGE_LOOP('',(#5029,#5030,#5031,#5032,#5033,#5034));
#2307=EDGE_LOOP('',(#5035));
#2308=EDGE_LOOP('',(#5036,#5037,#5038,#5039));
#2309=EDGE_LOOP('',(#5040,#5041,#5042,#5043));
#2310=EDGE_LOOP('',(#5044,#5045,#5046,#5047));
#2311=EDGE_LOOP('',(#5048,#5049,#5050,#5051));
#2312=EDGE_LOOP('',(#5052,#5053,#5054,#5055));
#2313=EDGE_LOOP('',(#5056,#5057,#5058,#5059));
#2314=EDGE_LOOP('',(#5060,#5061,#5062,#5063));
#2315=EDGE_LOOP('',(#5064,#5065,#5066,#5067,#5068));
#2316=EDGE_LOOP('',(#5069,#5070,#5071,#5072,#5073));
#2317=EDGE_LOOP('',(#5074,#5075,#5076,#5077,#5078,#5079,#5080,#5081,#5082,
#5083,#5084,#5085,#5086,#5087,#5088,#5089,#5090));
#2318=EDGE_LOOP('',(#5091,#5092));
#2319=EDGE_LOOP('',(#5093,#5094));
#2320=EDGE_LOOP('',(#5095,#5096,#5097,#5098,#5099,#5100,#5101,#5102));
#2321=EDGE_LOOP('',(#5103,#5104,#5105,#5106));
#2322=EDGE_LOOP('',(#5107,#5108));
#2323=EDGE_LOOP('',(#5109,#5110));
#2324=EDGE_LOOP('',(#5111,#5112,#5113,#5114));
#2325=EDGE_LOOP('',(#5115,#5116,#5117,#5118));
#2326=EDGE_LOOP('',(#5119,#5120,#5121,#5122,#5123,#5124,#5125));
#2327=EDGE_LOOP('',(#5126));
#2328=EDGE_LOOP('',(#5127,#5128,#5129,#5130,#5131,#5132,#5133));
#2329=EDGE_LOOP('',(#5134));
#2330=EDGE_LOOP('',(#5135,#5136,#5137,#5138));
#2331=EDGE_LOOP('',(#5139,#5140,#5141,#5142));
#2332=EDGE_LOOP('',(#5143,#5144,#5145,#5146,#5147,#5148,#5149,#5150));
#2333=EDGE_LOOP('',(#5151));
#2334=EDGE_LOOP('',(#5152,#5153,#5154,#5155,#5156));
#2335=EDGE_LOOP('',(#5157,#5158,#5159,#5160,#5161,#5162,#5163,#5164));
#2336=EDGE_LOOP('',(#5165));
#2337=EDGE_LOOP('',(#5166,#5167,#5168,#5169,#5170,#5171,#5172,#5173));
#2338=EDGE_LOOP('',(#5174,#5175,#5176,#5177,#5178,#5179,#5180,#5181));
#2339=EDGE_LOOP('',(#5182,#5183,#5184,#5185));
#2340=EDGE_LOOP('',(#5186,#5187,#5188,#5189));
#2341=EDGE_LOOP('',(#5190,#5191,#5192,#5193,#5194,#5195,#5196,#5197));
#2342=EDGE_LOOP('',(#5198));
#2343=EDGE_LOOP('',(#5199,#5200,#5201,#5202,#5203,#5204,#5205,#5206));
#2344=EDGE_LOOP('',(#5207));
#2345=EDGE_LOOP('',(#5208));
#2346=EDGE_LOOP('',(#5209));
#2347=EDGE_LOOP('',(#5210,#5211,#5212,#5213));
#2348=EDGE_LOOP('',(#5214,#5215,#5216,#5217));
#2349=EDGE_LOOP('',(#5218,#5219,#5220,#5221));
#2350=EDGE_LOOP('',(#5222,#5223,#5224,#5225));
#2351=EDGE_LOOP('',(#5226,#5227,#5228,#5229));
#2352=EDGE_LOOP('',(#5230,#5231,#5232,#5233));
#2353=EDGE_LOOP('',(#5234,#5235,#5236,#5237));
#2354=EDGE_LOOP('',(#5238,#5239,#5240,#5241,#5242,#5243));
#2355=EDGE_LOOP('',(#5244));
#2356=EDGE_LOOP('',(#5245,#5246,#5247,#5248));
#2357=EDGE_LOOP('',(#5249,#5250,#5251,#5252,#5253,#5254));
#2358=EDGE_LOOP('',(#5255));
#2359=EDGE_LOOP('',(#5256,#5257,#5258,#5259));
#2360=EDGE_LOOP('',(#5260,#5261,#5262,#5263));
#2361=EDGE_LOOP('',(#5264,#5265,#5266,#5267));
#2362=EDGE_LOOP('',(#5268,#5269,#5270));
#2363=EDGE_LOOP('',(#5271,#5272,#5273));
#2364=EDGE_LOOP('',(#5274,#5275,#5276,#5277));
#2365=EDGE_LOOP('',(#5278,#5279,#5280,#5281));
#2366=EDGE_LOOP('',(#5282,#5283,#5284,#5285));
#2367=EDGE_LOOP('',(#5286,#5287,#5288,#5289));
#2368=EDGE_LOOP('',(#5290,#5291,#5292,#5293));
#2369=EDGE_LOOP('',(#5294,#5295,#5296,#5297));
#2370=EDGE_LOOP('',(#5298,#5299,#5300,#5301));
#2371=EDGE_LOOP('',(#5302,#5303,#5304,#5305,#5306));
#2372=EDGE_LOOP('',(#5307,#5308,#5309,#5310,#5311));
#2373=EDGE_LOOP('',(#5312,#5313,#5314,#5315,#5316,#5317,#5318,#5319,#5320,
#5321,#5322,#5323,#5324,#5325,#5326,#5327,#5328,#5329,#5330,#5331,#5332));
#2374=EDGE_LOOP('',(#5333,#5334));
#2375=EDGE_LOOP('',(#5335,#5336));
#2376=EDGE_LOOP('',(#5337,#5338,#5339,#5340));
#2377=EDGE_LOOP('',(#5341,#5342,#5343,#5344));
#2378=EDGE_LOOP('',(#5345,#5346,#5347,#5348));
#2379=EDGE_LOOP('',(#5349));
#2380=EDGE_LOOP('',(#5350,#5351,#5352,#5353,#5354,#5355,#5356,#5357));
#2381=EDGE_LOOP('',(#5358,#5359,#5360,#5361));
#2382=EDGE_LOOP('',(#5362,#5363));
#2383=EDGE_LOOP('',(#5364,#5365));
#2384=EDGE_LOOP('',(#5366,#5367,#5368,#5369));
#2385=EDGE_LOOP('',(#5370,#5371,#5372,#5373));
#2386=EDGE_LOOP('',(#5374,#5375,#5376,#5377,#5378,#5379,#5380,#5381,#5382));
#2387=EDGE_LOOP('',(#5383));
#2388=EDGE_LOOP('',(#5384,#5385,#5386,#5387,#5388,#5389,#5390,#5391,#5392));
#2389=EDGE_LOOP('',(#5393));
#2390=EDGE_LOOP('',(#5394,#5395,#5396,#5397));
#2391=EDGE_LOOP('',(#5398,#5399,#5400,#5401));
#2392=EDGE_LOOP('',(#5402,#5403,#5404,#5405,#5406,#5407,#5408,#5409));
#2393=EDGE_LOOP('',(#5410));
#2394=EDGE_LOOP('',(#5411,#5412,#5413,#5414,#5415));
#2395=EDGE_LOOP('',(#5416,#5417,#5418,#5419,#5420,#5421,#5422,#5423));
#2396=EDGE_LOOP('',(#5424));
#2397=EDGE_LOOP('',(#5425,#5426,#5427,#5428,#5429,#5430,#5431,#5432));
#2398=EDGE_LOOP('',(#5433,#5434,#5435,#5436,#5437,#5438,#5439,#5440));
#2399=EDGE_LOOP('',(#5441,#5442,#5443,#5444));
#2400=EDGE_LOOP('',(#5445,#5446,#5447,#5448));
#2401=EDGE_LOOP('',(#5449,#5450,#5451,#5452,#5453,#5454,#5455,#5456));
#2402=EDGE_LOOP('',(#5457));
#2403=EDGE_LOOP('',(#5458,#5459,#5460,#5461,#5462,#5463,#5464,#5465));
#2404=EDGE_LOOP('',(#5466));
#2405=EDGE_LOOP('',(#5467));
#2406=EDGE_LOOP('',(#5468));
#2407=EDGE_LOOP('',(#5469,#5470,#5471,#5472));
#2408=EDGE_LOOP('',(#5473,#5474,#5475,#5476));
#2409=EDGE_LOOP('',(#5477,#5478,#5479,#5480));
#2410=EDGE_LOOP('',(#5481,#5482,#5483,#5484));
#2411=EDGE_LOOP('',(#5485,#5486,#5487,#5488));
#2412=EDGE_LOOP('',(#5489,#5490,#5491,#5492));
#2413=EDGE_LOOP('',(#5493,#5494,#5495,#5496));
#2414=EDGE_LOOP('',(#5497,#5498,#5499,#5500,#5501,#5502));
#2415=EDGE_LOOP('',(#5503));
#2416=EDGE_LOOP('',(#5504,#5505,#5506,#5507));
#2417=EDGE_LOOP('',(#5508,#5509,#5510,#5511,#5512,#5513));
#2418=EDGE_LOOP('',(#5514));
#2419=EDGE_LOOP('',(#5515,#5516,#5517,#5518));
#2420=EDGE_LOOP('',(#5519,#5520,#5521,#5522));
#2421=EDGE_LOOP('',(#5523,#5524,#5525,#5526));
#2422=EDGE_LOOP('',(#5527,#5528,#5529,#5530));
#2423=EDGE_LOOP('',(#5531,#5532,#5533,#5534));
#2424=EDGE_LOOP('',(#5535));
#2425=EDGE_LOOP('',(#5536,#5537,#5538));
#2426=EDGE_LOOP('',(#5539,#5540,#5541));
#2427=EDGE_LOOP('',(#5542,#5543,#5544,#5545));
#2428=EDGE_LOOP('',(#5546,#5547,#5548,#5549));
#2429=EDGE_LOOP('',(#5550,#5551,#5552,#5553));
#2430=EDGE_LOOP('',(#5554,#5555,#5556,#5557));
#2431=EDGE_LOOP('',(#5558,#5559,#5560,#5561));
#2432=EDGE_LOOP('',(#5562));
#2433=EDGE_LOOP('',(#5563,#5564,#5565,#5566));
#2434=EDGE_LOOP('',(#5567));
#2435=EDGE_LOOP('',(#5568));
#2436=EDGE_LOOP('',(#5569,#5570,#5571,#5572));
#2437=EDGE_LOOP('',(#5573));
#2438=EDGE_LOOP('',(#5574,#5575,#5576,#5577));
#2439=EDGE_LOOP('',(#5578,#5579,#5580,#5581));
#2440=EDGE_LOOP('',(#5582));
#2441=EDGE_LOOP('',(#5583,#5584,#5585,#5586));
#2442=EDGE_LOOP('',(#5587,#5588,#5589,#5590));
#2443=EDGE_LOOP('',(#5591));
#2444=EDGE_LOOP('',(#5592,#5593,#5594,#5595));
#2445=EDGE_LOOP('',(#5596,#5597,#5598,#5599));
#2446=EDGE_LOOP('',(#5600,#5601,#5602,#5603));
#2447=EDGE_LOOP('',(#5604));
#2448=EDGE_LOOP('',(#5605,#5606,#5607,#5608));
#2449=EDGE_LOOP('',(#5609));
#2450=EDGE_LOOP('',(#5610,#5611,#5612,#5613));
#2451=EDGE_LOOP('',(#5614));
#2452=EDGE_LOOP('',(#5615,#5616,#5617,#5618));
#2453=EDGE_LOOP('',(#5619,#5620,#5621,#5622));
#2454=EDGE_LOOP('',(#5623));
#2455=EDGE_LOOP('',(#5624,#5625,#5626,#5627));
#2456=EDGE_LOOP('',(#5628,#5629,#5630,#5631));
#2457=EDGE_LOOP('',(#5632,#5633,#5634,#5635));
#2458=EDGE_LOOP('',(#5636,#5637,#5638,#5639));
#2459=EDGE_LOOP('',(#5640));
#2460=EDGE_LOOP('',(#5641,#5642,#5643,#5644));
#2461=EDGE_LOOP('',(#5645));
#2462=EDGE_LOOP('',(#5646));
#2463=EDGE_LOOP('',(#5647,#5648,#5649,#5650));
#2464=EDGE_LOOP('',(#5651));
#2465=EDGE_LOOP('',(#5652,#5653,#5654,#5655));
#2466=EDGE_LOOP('',(#5656,#5657,#5658,#5659));
#2467=EDGE_LOOP('',(#5660));
#2468=EDGE_LOOP('',(#5661,#5662,#5663,#5664));
#2469=EDGE_LOOP('',(#5665,#5666,#5667,#5668));
#2470=EDGE_LOOP('',(#5669));
#2471=EDGE_LOOP('',(#5670,#5671,#5672,#5673));
#2472=EDGE_LOOP('',(#5674,#5675,#5676,#5677));
#2473=EDGE_LOOP('',(#5678,#5679,#5680,#5681));
#2474=EDGE_LOOP('',(#5682));
#2475=EDGE_LOOP('',(#5683,#5684,#5685,#5686));
#2476=EDGE_LOOP('',(#5687));
#2477=EDGE_LOOP('',(#5688,#5689,#5690,#5691));
#2478=EDGE_LOOP('',(#5692));
#2479=EDGE_LOOP('',(#5693,#5694,#5695,#5696));
#2480=EDGE_LOOP('',(#5697,#5698,#5699,#5700));
#2481=EDGE_LOOP('',(#5701));
#2482=EDGE_LOOP('',(#5702,#5703,#5704,#5705));
#2483=EDGE_LOOP('',(#5706,#5707,#5708,#5709));
#2484=EDGE_LOOP('',(#5710,#5711,#5712,#5713));
#2485=EDGE_LOOP('',(#5714,#5715,#5716,#5717));
#2486=EDGE_LOOP('',(#5718));
#2487=EDGE_LOOP('',(#5719,#5720,#5721,#5722));
#2488=EDGE_LOOP('',(#5723));
#2489=EDGE_LOOP('',(#5724));
#2490=EDGE_LOOP('',(#5725,#5726,#5727,#5728));
#2491=EDGE_LOOP('',(#5729));
#2492=EDGE_LOOP('',(#5730,#5731,#5732,#5733));
#2493=EDGE_LOOP('',(#5734,#5735,#5736,#5737));
#2494=EDGE_LOOP('',(#5738));
#2495=EDGE_LOOP('',(#5739,#5740,#5741,#5742));
#2496=EDGE_LOOP('',(#5743,#5744,#5745,#5746));
#2497=EDGE_LOOP('',(#5747));
#2498=EDGE_LOOP('',(#5748,#5749,#5750,#5751));
#2499=EDGE_LOOP('',(#5752,#5753,#5754,#5755));
#2500=EDGE_LOOP('',(#5756,#5757,#5758,#5759));
#2501=EDGE_LOOP('',(#5760));
#2502=EDGE_LOOP('',(#5761,#5762,#5763,#5764));
#2503=EDGE_LOOP('',(#5765));
#2504=EDGE_LOOP('',(#5766,#5767,#5768,#5769));
#2505=EDGE_LOOP('',(#5770));
#2506=EDGE_LOOP('',(#5771,#5772,#5773,#5774));
#2507=EDGE_LOOP('',(#5775,#5776,#5777,#5778));
#2508=EDGE_LOOP('',(#5779));
#2509=EDGE_LOOP('',(#5780,#5781,#5782,#5783));
#2510=EDGE_LOOP('',(#5784,#5785,#5786,#5787));
#2511=EDGE_LOOP('',(#5788,#5789,#5790,#5791));
#2512=EDGE_LOOP('',(#5792,#5793,#5794,#5795));
#2513=EDGE_LOOP('',(#5796,#5797,#5798,#5799));
#2514=EDGE_LOOP('',(#5800,#5801,#5802,#5803,#5804,#5805));
#2515=EDGE_LOOP('',(#5806));
#2516=EDGE_LOOP('',(#5807,#5808,#5809,#5810));
#2517=EDGE_LOOP('',(#5811,#5812,#5813,#5814,#5815,#5816));
#2518=EDGE_LOOP('',(#5817));
#2519=EDGE_LOOP('',(#5818,#5819,#5820,#5821));
#2520=EDGE_LOOP('',(#5822,#5823,#5824,#5825));
#2521=EDGE_LOOP('',(#5826,#5827,#5828,#5829,#5830,#5831,#5832,#5833));
#2522=EDGE_LOOP('',(#5834,#5835,#5836,#5837,#5838,#5839,#5840,#5841));
#2523=EDGE_LOOP('',(#5842,#5843,#5844,#5845));
#2524=EDGE_LOOP('',(#5846,#5847,#5848,#5849));
#2525=EDGE_LOOP('',(#5850));
#2526=EDGE_LOOP('',(#5851,#5852,#5853,#5854));
#2527=EDGE_LOOP('',(#5855));
#2528=EDGE_LOOP('',(#5856,#5857,#5858,#5859));
#2529=EDGE_LOOP('',(#5860));
#2530=EDGE_LOOP('',(#5861));
#2531=EDGE_LOOP('',(#5862,#5863,#5864,#5865,#5866));
#2532=EDGE_LOOP('',(#5867,#5868,#5869,#5870,#5871));
#2533=EDGE_LOOP('',(#5872,#5873,#5874));
#2534=EDGE_LOOP('',(#5875,#5876,#5877,#5878));
#2535=EDGE_LOOP('',(#5879,#5880));
#2536=EDGE_LOOP('',(#5881,#5882));
#2537=EDGE_LOOP('',(#5883));
#2538=EDGE_LOOP('',(#5884,#5885,#5886,#5887));
#2539=EDGE_LOOP('',(#5888,#5889,#5890,#5891));
#2540=EDGE_LOOP('',(#5892,#5893,#5894,#5895));
#2541=EDGE_LOOP('',(#5896,#5897,#5898,#5899));
#2542=EDGE_LOOP('',(#5900));
#2543=EDGE_LOOP('',(#5901,#5902,#5903,#5904));
#2544=EDGE_LOOP('',(#5905,#5906,#5907,#5908));
#2545=EDGE_LOOP('',(#5909));
#2546=EDGE_LOOP('',(#5910,#5911,#5912,#5913));
#2547=EDGE_LOOP('',(#5914,#5915,#5916,#5917));
#2548=EDGE_LOOP('',(#5918,#5919,#5920,#5921));
#2549=EDGE_LOOP('',(#5922,#5923,#5924,#5925));
#2550=EDGE_LOOP('',(#5926,#5927,#5928,#5929,#5930,#5931,#5932,#5933,#5934,
#5935,#5936,#5937));
#2551=EDGE_LOOP('',(#5938,#5939,#5940,#5941));
#2552=EDGE_LOOP('',(#5942,#5943,#5944,#5945));
#2553=EDGE_LOOP('',(#5946,#5947,#5948,#5949));
#2554=EDGE_LOOP('',(#5950,#5951,#5952,#5953));
#2555=EDGE_LOOP('',(#5954,#5955,#5956,#5957));
#2556=EDGE_LOOP('',(#5958));
#2557=EDGE_LOOP('',(#5959,#5960,#5961,#5962));
#2558=EDGE_LOOP('',(#5963,#5964,#5965,#5966));
#2559=EDGE_LOOP('',(#5967));
#2560=EDGE_LOOP('',(#5968,#5969,#5970,#5971));
#2561=EDGE_LOOP('',(#5972,#5973,#5974,#5975));
#2562=EDGE_LOOP('',(#5976));
#2563=EDGE_LOOP('',(#5977,#5978,#5979,#5980));
#2564=EDGE_LOOP('',(#5981,#5982,#5983,#5984));
#2565=EDGE_LOOP('',(#5985));
#2566=EDGE_LOOP('',(#5986,#5987,#5988,#5989));
#2567=EDGE_LOOP('',(#5990,#5991,#5992,#5993,#5994,#5995,#5996,#5997));
#2568=EDGE_LOOP('',(#5998,#5999,#6000,#6001));
#2569=EDGE_LOOP('',(#6002,#6003,#6004,#6005,#6006,#6007,#6008,#6009));
#2570=EDGE_LOOP('',(#6010,#6011,#6012,#6013));
#2571=EDGE_LOOP('',(#6014,#6015,#6016,#6017));
#2572=EDGE_LOOP('',(#6018,#6019,#6020,#6021));
#2573=EDGE_LOOP('',(#6022,#6023,#6024,#6025));
#2574=EDGE_LOOP('',(#6026));
#2575=EDGE_LOOP('',(#6027,#6028,#6029,#6030));
#2576=EDGE_LOOP('',(#6031));
#2577=EDGE_LOOP('',(#6032,#6033,#6034,#6035));
#2578=EDGE_LOOP('',(#6036,#6037,#6038,#6039,#6040));
#2579=EDGE_LOOP('',(#6041,#6042,#6043,#6044,#6045));
#2580=EDGE_LOOP('',(#6046,#6047,#6048,#6049));
#2581=EDGE_LOOP('',(#6050,#6051,#6052,#6053,#6054,#6055,#6056,#6057));
#2582=EDGE_LOOP('',(#6058,#6059,#6060,#6061,#6062,#6063));
#2583=EDGE_LOOP('',(#6064,#6065,#6066,#6067,#6068,#6069,#6070,#6071,#6072,
#6073,#6074,#6075));
#2584=EDGE_LOOP('',(#6076,#6077));
#2585=EDGE_LOOP('',(#6078,#6079));
#2586=EDGE_LOOP('',(#6080,#6081,#6082,#6083));
#2587=EDGE_LOOP('',(#6084,#6085,#6086,#6087));
#2588=EDGE_LOOP('',(#6088,#6089,#6090,#6091));
#2589=EDGE_LOOP('',(#6092,#6093,#6094,#6095));
#2590=EDGE_LOOP('',(#6096));
#2591=EDGE_LOOP('',(#6097,#6098,#6099,#6100));
#2592=EDGE_LOOP('',(#6101));
#2593=EDGE_LOOP('',(#6102,#6103,#6104,#6105,#6106,#6107));
#2594=EDGE_LOOP('',(#6108,#6109,#6110,#6111));
#2595=EDGE_LOOP('',(#6112,#6113,#6114,#6115));
#2596=EDGE_LOOP('',(#6116,#6117,#6118,#6119));
#2597=EDGE_LOOP('',(#6120,#6121,#6122,#6123));
#2598=EDGE_LOOP('',(#6124,#6125,#6126,#6127,#6128,#6129));
#2599=EDGE_LOOP('',(#6130));
#2600=EDGE_LOOP('',(#6131,#6132,#6133,#6134,#6135,#6136));
#2601=EDGE_LOOP('',(#6137));
#2602=EDGE_LOOP('',(#6138,#6139,#6140,#6141,#6142));
#2603=EDGE_LOOP('',(#6143,#6144,#6145,#6146,#6147));
#2604=EDGE_LOOP('',(#6148,#6149,#6150,#6151,#6152,#6153,#6154,#6155,#6156,
#6157));
#2605=EDGE_LOOP('',(#6158,#6159,#6160,#6161));
#2606=EDGE_LOOP('',(#6162,#6163,#6164,#6165));
#2607=EDGE_LOOP('',(#6166,#6167,#6168,#6169));
#2608=EDGE_LOOP('',(#6170,#6171,#6172,#6173,#6174,#6175,#6176,#6177,#6178,
#6179,#6180,#6181));
#2609=EDGE_LOOP('',(#6182,#6183));
#2610=EDGE_LOOP('',(#6184,#6185));
#2611=EDGE_LOOP('',(#6186,#6187,#6188));
#2612=EDGE_LOOP('',(#6189,#6190,#6191,#6192));
#2613=EDGE_LOOP('',(#6193,#6194,#6195,#6196));
#2614=EDGE_LOOP('',(#6197,#6198,#6199,#6200));
#2615=EDGE_LOOP('',(#6201,#6202));
#2616=EDGE_LOOP('',(#6203,#6204,#6205,#6206,#6207,#6208,#6209,#6210,#6211));
#2617=EDGE_LOOP('',(#6212,#6213,#6214,#6215));
#2618=EDGE_LOOP('',(#6216,#6217));
#2619=EDGE_LOOP('',(#6218,#6219,#6220,#6221,#6222,#6223));
#2620=EDGE_LOOP('',(#6224));
#2621=EDGE_LOOP('',(#6225,#6226,#6227,#6228,#6229,#6230));
#2622=EDGE_LOOP('',(#6231));
#2623=EDGE_LOOP('',(#6232,#6233,#6234,#6235));
#2624=EDGE_LOOP('',(#6236,#6237,#6238,#6239,#6240));
#2625=EDGE_LOOP('',(#6241,#6242,#6243,#6244,#6245,#6246,#6247,#6248));
#2626=EDGE_LOOP('',(#6249));
#2627=EDGE_LOOP('',(#6250,#6251,#6252,#6253));
#2628=EDGE_LOOP('',(#6254,#6255,#6256,#6257,#6258,#6259,#6260,#6261,#6262));
#2629=EDGE_LOOP('',(#6263));
#2630=EDGE_LOOP('',(#6264,#6265,#6266));
#2631=EDGE_LOOP('',(#6267,#6268,#6269,#6270,#6271,#6272,#6273,#6274,#6275,
#6276,#6277,#6278));
#2632=EDGE_LOOP('',(#6279,#6280,#6281,#6282,#6283,#6284,#6285,#6286));
#2633=EDGE_LOOP('',(#6287,#6288,#6289,#6290));
#2634=EDGE_LOOP('',(#6291,#6292,#6293));
#2635=EDGE_LOOP('',(#6294,#6295,#6296,#6297,#6298,#6299));
#2636=EDGE_LOOP('',(#6300));
#2637=EDGE_LOOP('',(#6301,#6302,#6303,#6304,#6305,#6306));
#2638=EDGE_LOOP('',(#6307));
#2639=EDGE_LOOP('',(#6308));
#2640=EDGE_LOOP('',(#6309));
#2641=EDGE_LOOP('',(#6310,#6311,#6312,#6313));
#2642=EDGE_LOOP('',(#6314,#6315,#6316,#6317));
#2643=EDGE_LOOP('',(#6318,#6319,#6320,#6321));
#2644=EDGE_LOOP('',(#6322,#6323,#6324,#6325));
#2645=EDGE_LOOP('',(#6326,#6327,#6328,#6329,#6330,#6331));
#2646=EDGE_LOOP('',(#6332,#6333,#6334,#6335,#6336,#6337,#6338,#6339));
#2647=EDGE_LOOP('',(#6340,#6341,#6342,#6343));
#2648=EDGE_LOOP('',(#6344,#6345,#6346,#6347));
#2649=EDGE_LOOP('',(#6348,#6349,#6350,#6351));
#2650=EDGE_LOOP('',(#6352,#6353,#6354,#6355));
#2651=EDGE_LOOP('',(#6356,#6357,#6358));
#2652=EDGE_LOOP('',(#6359,#6360,#6361,#6362));
#2653=EDGE_LOOP('',(#6363));
#2654=EDGE_LOOP('',(#6364,#6365,#6366,#6367));
#2655=EDGE_LOOP('',(#6368,#6369,#6370,#6371));
#2656=EDGE_LOOP('',(#6372,#6373,#6374,#6375));
#2657=EDGE_LOOP('',(#6376));
#2658=EDGE_LOOP('',(#6377,#6378,#6379,#6380));
#2659=EDGE_LOOP('',(#6381));
#2660=EDGE_LOOP('',(#6382));
#2661=EDGE_LOOP('',(#6383,#6384,#6385,#6386));
#2662=EDGE_LOOP('',(#6387));
#2663=EDGE_LOOP('',(#6388,#6389,#6390,#6391));
#2664=EDGE_LOOP('',(#6392,#6393,#6394,#6395));
#2665=EDGE_LOOP('',(#6396));
#2666=EDGE_LOOP('',(#6397,#6398,#6399,#6400));
#2667=EDGE_LOOP('',(#6401,#6402,#6403,#6404));
#2668=EDGE_LOOP('',(#6405));
#2669=EDGE_LOOP('',(#6406,#6407,#6408,#6409));
#2670=EDGE_LOOP('',(#6410,#6411,#6412,#6413));
#2671=EDGE_LOOP('',(#6414,#6415,#6416,#6417));
#2672=EDGE_LOOP('',(#6418));
#2673=EDGE_LOOP('',(#6419,#6420,#6421,#6422));
#2674=EDGE_LOOP('',(#6423));
#2675=EDGE_LOOP('',(#6424,#6425,#6426,#6427));
#2676=EDGE_LOOP('',(#6428));
#2677=EDGE_LOOP('',(#6429,#6430,#6431,#6432));
#2678=EDGE_LOOP('',(#6433,#6434,#6435,#6436));
#2679=EDGE_LOOP('',(#6437));
#2680=EDGE_LOOP('',(#6438,#6439,#6440,#6441));
#2681=CIRCLE('',#7063,22.);
#2682=CIRCLE('',#7064,2.);
#2683=CIRCLE('',#7065,20.);
#2684=CIRCLE('',#7066,2.);
#2685=CIRCLE('',#7068,20.);
#2686=CIRCLE('',#7069,2.);
#2687=CIRCLE('',#7070,22.);
#2688=CIRCLE('',#7071,2.);
#2689=CIRCLE('',#7073,2.);
#2690=CIRCLE('',#7074,2.);
#2691=CIRCLE('',#7075,2.);
#2692=CIRCLE('',#7077,1.5);
#2693=CIRCLE('',#7078,1.5);
#2694=CIRCLE('',#7080,1.5);
#2695=CIRCLE('',#7081,1.5);
#2696=CIRCLE('',#7083,56.4897440054506);
#2697=CIRCLE('',#7084,56.4897440054506);
#2698=CIRCLE('',#7088,25.);
#2699=CIRCLE('',#7089,4.54881469766181);
#2700=CIRCLE('',#7090,25.);
#2701=CIRCLE('',#7095,25.);
#2702=CIRCLE('',#7097,25.);
#2703=CIRCLE('',#7098,4.54881469766181);
#2704=CIRCLE('',#7100,163.25688730188);
#2705=CIRCLE('',#7101,163.25688730188);
#2706=CIRCLE('',#7102,163.25688730188);
#2707=CIRCLE('',#7103,163.25688730188);
#2708=CIRCLE('',#7111,161.25688730188);
#2709=CIRCLE('',#7112,54.4897440054506);
#2710=CIRCLE('',#7113,4.);
#2711=CIRCLE('',#7115,4.);
#2712=CIRCLE('',#7116,54.4897440054506);
#2713=CIRCLE('',#7117,161.25688730188);
#2714=CIRCLE('',#7119,8.);
#2715=CIRCLE('',#7121,8.00000000000001);
#2716=CIRCLE('',#7128,2.);
#2717=CIRCLE('',#7129,2.);
#2718=CIRCLE('',#7131,2.);
#2719=CIRCLE('',#7132,2.);
#2720=CIRCLE('',#7134,2.);
#2721=CIRCLE('',#7135,2.);
#2722=CIRCLE('',#7137,2.);
#2723=CIRCLE('',#7139,2.);
#2724=CIRCLE('',#7142,2.);
#2725=CIRCLE('',#7144,2.);
#2726=CIRCLE('',#7145,2.);
#2727=CIRCLE('',#7147,2.);
#2728=CIRCLE('',#7149,2.);
#2729=CIRCLE('',#7150,2.);
#2730=CIRCLE('',#7152,2.);
#2731=CIRCLE('',#7154,2.);
#2732=CIRCLE('',#7156,2.);
#2733=CIRCLE('',#7158,2.);
#2734=CIRCLE('',#7160,2.);
#2735=CIRCLE('',#7162,2.00000000000001);
#2736=CIRCLE('',#7164,2.);
#2737=CIRCLE('',#7166,2.);
#2738=CIRCLE('',#7168,2.);
#2739=CIRCLE('',#7170,2.);
#2740=CIRCLE('',#7172,2.);
#2741=CIRCLE('',#7174,2.);
#2742=CIRCLE('',#7176,2.);
#2743=CIRCLE('',#7178,2.);
#2744=CIRCLE('',#7180,2.);
#2745=CIRCLE('',#7182,2.);
#2746=CIRCLE('',#7185,2.);
#2747=CIRCLE('',#7201,1.5);
#2748=CIRCLE('',#7202,1.5);
#2749=CIRCLE('',#7204,1.);
#2750=CIRCLE('',#7205,1.);
#2751=CIRCLE('',#7207,1.);
#2752=CIRCLE('',#7208,1.);
#2753=CIRCLE('',#7210,1.);
#2754=CIRCLE('',#7211,1.);
#2755=CIRCLE('',#7213,1.5);
#2756=CIRCLE('',#7215,1.5);
#2757=CIRCLE('',#7217,12.7565008166693);
#2758=CIRCLE('',#7218,12.8874008156035);
#2759=CIRCLE('',#7219,12.8874008156035);
#2760=CIRCLE('',#7222,1.);
#2761=CIRCLE('',#7224,1.);
#2762=CIRCLE('',#7227,12.9921312051728);
#2763=CIRCLE('',#7229,35.);
#2764=CIRCLE('',#7230,35.);
#2765=CIRCLE('',#7232,26.);
#2766=CIRCLE('',#7233,26.);
#2767=CIRCLE('',#7240,1.);
#2768=CIRCLE('',#7241,1.);
#2769=CIRCLE('',#7244,1.);
#2770=CIRCLE('',#7245,1.);
#2771=CIRCLE('',#7251,1.);
#2772=CIRCLE('',#7252,1.);
#2773=CIRCLE('',#7254,1.);
#2774=CIRCLE('',#7255,1.);
#2775=CIRCLE('',#7265,3.);
#2776=CIRCLE('',#7266,3.);
#2777=CIRCLE('',#7269,3.);
#2778=CIRCLE('',#7270,3.);
#2779=CIRCLE('',#7276,1.35);
#2780=CIRCLE('',#7277,1.35);
#2781=CIRCLE('',#7279,0.900000000000001);
#2782=CIRCLE('',#7280,0.900000000000001);
#2783=CIRCLE('',#7282,0.900000000000001);
#2784=CIRCLE('',#7283,0.900000000000001);
#2785=CIRCLE('',#7285,0.900000000000001);
#2786=CIRCLE('',#7286,0.900000000000001);
#2787=CIRCLE('',#7288,1.35);
#2788=CIRCLE('',#7290,1.35);
#2789=CIRCLE('',#7292,11.4453313393709);
#2790=CIRCLE('',#7293,11.5986607340431);
#2791=CIRCLE('',#7294,11.5986607340431);
#2792=CIRCLE('',#7296,31.5);
#2793=CIRCLE('',#7297,31.5);
#2794=CIRCLE('',#7300,11.6929180846555);
#2795=CIRCLE('',#7302,23.4);
#2796=CIRCLE('',#7303,23.4);
#2797=CIRCLE('',#7305,9.44563594905814);
#2798=CIRCLE('',#7307,15.4750964764976);
#2799=CIRCLE('',#7308,10.);
#2800=CIRCLE('',#7310,10.);
#2801=CIRCLE('',#7311,15.4750964764976);
#2802=CIRCLE('',#7315,0.9);
#2803=CIRCLE('',#7316,0.9);
#2804=CIRCLE('',#7319,0.9);
#2805=CIRCLE('',#7320,0.9);
#2806=CIRCLE('',#7326,0.9);
#2807=CIRCLE('',#7327,0.9);
#2808=CIRCLE('',#7328,0.9);
#2809=CIRCLE('',#7329,0.9);
#2810=CIRCLE('',#7331,0.9);
#2811=CIRCLE('',#7332,0.9);
#2812=CIRCLE('',#7333,0.9);
#2813=CIRCLE('',#7334,0.9);
#2814=CIRCLE('',#7345,2.7);
#2815=CIRCLE('',#7346,2.7);
#2816=CIRCLE('',#7349,2.7);
#2817=CIRCLE('',#7350,2.7);
#2818=CIRCLE('',#7361,1.2);
#2819=CIRCLE('',#7362,1.2);
#2820=CIRCLE('',#7364,0.800000000000001);
#2821=CIRCLE('',#7365,0.800000000000001);
#2822=CIRCLE('',#7367,0.800000000000001);
#2823=CIRCLE('',#7368,0.800000000000001);
#2824=CIRCLE('',#7370,0.800000000000001);
#2825=CIRCLE('',#7371,0.800000000000001);
#2826=CIRCLE('',#7373,1.2);
#2827=CIRCLE('',#7375,1.2);
#2828=CIRCLE('',#7377,10.169681257704);
#2829=CIRCLE('',#7378,10.3099206524828);
#2830=CIRCLE('',#7379,10.3099206524828);
#2831=CIRCLE('',#7381,16.7532667406203);
#2832=CIRCLE('',#7383,16.7532667406203);
#2833=CIRCLE('',#7385,8.16998586739121);
#2834=CIRCLE('',#7387,28.);
#2835=CIRCLE('',#7388,28.);
#2836=CIRCLE('',#7391,10.3937049641382);
#2837=CIRCLE('',#7393,20.8);
#2838=CIRCLE('',#7394,20.8);
#2839=CIRCLE('',#7397,4.06015460582196);
#2840=CIRCLE('',#7398,22.);
#2841=CIRCLE('',#7399,10.);
#2842=CIRCLE('',#7401,22.);
#2843=CIRCLE('',#7402,4.06015460582196);
#2844=CIRCLE('',#7403,10.);
#2845=CIRCLE('',#7407,0.8);
#2846=CIRCLE('',#7408,0.8);
#2847=CIRCLE('',#7411,0.8);
#2848=CIRCLE('',#7412,0.8);
#2849=CIRCLE('',#7418,0.8);
#2850=CIRCLE('',#7419,0.8);
#2851=CIRCLE('',#7420,0.8);
#2852=CIRCLE('',#7421,0.8);
#2853=CIRCLE('',#7423,0.8);
#2854=CIRCLE('',#7424,0.8);
#2855=CIRCLE('',#7425,0.8);
#2856=CIRCLE('',#7426,0.8);
#2857=CIRCLE('',#7437,2.4);
#2858=CIRCLE('',#7438,2.4);
#2859=CIRCLE('',#7441,2.4);
#2860=CIRCLE('',#7442,2.4);
#2861=CIRCLE('',#7456,1.825);
#2862=CIRCLE('',#7457,1.825);
#2863=CIRCLE('',#7459,1.095);
#2864=CIRCLE('',#7460,1.095);
#2865=CIRCLE('',#7462,2.92);
#2866=CIRCLE('',#7463,2.92);
#2867=CIRCLE('',#7467,2.19);
#2868=CIRCLE('',#7470,2.19);
#2869=CIRCLE('',#7476,0.729999999999999);
#2870=CIRCLE('',#7477,0.729999999999999);
#2871=CIRCLE('',#7479,1.46);
#2872=CIRCLE('',#7480,1.46);
#2873=CIRCLE('',#7482,1.825);
#2874=CIRCLE('',#7483,1.825);
#2875=CIRCLE('',#7495,1.825);
#2876=CIRCLE('',#7496,1.825);
#2877=CIRCLE('',#7498,1.095);
#2878=CIRCLE('',#7499,1.095);
#2879=CIRCLE('',#7501,2.92);
#2880=CIRCLE('',#7502,2.92);
#2881=CIRCLE('',#7506,2.19);
#2882=CIRCLE('',#7509,2.19);
#2883=CIRCLE('',#7515,0.730000000000001);
#2884=CIRCLE('',#7516,0.730000000000001);
#2885=CIRCLE('',#7518,1.46);
#2886=CIRCLE('',#7519,1.46);
#2887=CIRCLE('',#7521,1.825);
#2888=CIRCLE('',#7522,1.825);
#2889=CIRCLE('',#7534,2.5);
#2890=CIRCLE('',#7535,2.5);
#2891=CIRCLE('',#7537,1.5);
#2892=CIRCLE('',#7538,1.5);
#2893=CIRCLE('',#7540,4.);
#2894=CIRCLE('',#7541,4.);
#2895=CIRCLE('',#7545,3.);
#2896=CIRCLE('',#7548,3.);
#2897=CIRCLE('',#7554,1.);
#2898=CIRCLE('',#7555,1.);
#2899=CIRCLE('',#7557,2.);
#2900=CIRCLE('',#7558,2.);
#2901=CIRCLE('',#7560,2.50000000000001);
#2902=CIRCLE('',#7561,2.50000000000001);
#2903=CIRCLE('',#7570,1.);
#2904=CIRCLE('',#7571,1.);
#2905=CIRCLE('',#7573,1.);
#2906=CIRCLE('',#7574,1.);
#2907=CIRCLE('',#7576,1.);
#2908=CIRCLE('',#7577,1.);
#2909=CIRCLE('',#7597,1.);
#2910=CIRCLE('',#7599,1.);
#2911=CIRCLE('',#7600,4.44993914281691);
#2912=CIRCLE('',#7601,4.54815386259491);
#2913=CIRCLE('',#7603,20.);
#2914=CIRCLE('',#7604,20.);
#2915=CIRCLE('',#7620,1.);
#2916=CIRCLE('',#7621,1.);
#2917=CIRCLE('',#7623,1.5);
#2918=CIRCLE('',#7624,1.5);
#2919=CIRCLE('',#7626,1.5);
#2920=CIRCLE('',#7627,1.5);
#2921=CIRCLE('',#7629,1.5);
#2922=CIRCLE('',#7630,1.5);
#2923=CIRCLE('',#7632,17.5);
#2924=CIRCLE('',#7633,17.1097742533325);
#2925=CIRCLE('',#7634,7.08872343937892);
#2926=CIRCLE('',#7635,17.1097742533325);
#2927=CIRCLE('',#7636,17.5);
#2928=CIRCLE('',#7637,17.1097742533325);
#2929=CIRCLE('',#7638,16.9253361239603);
#2930=CIRCLE('',#7639,17.1097742533325);
#2931=CIRCLE('',#7640,17.3675981074726);
#2932=CIRCLE('',#7641,16.4471056942753);
#2933=CIRCLE('',#7642,17.3675981074726);
#2934=CIRCLE('',#7643,16.4471056942753);
#2935=CIRCLE('',#7644,17.0367250374008);
#2936=CIRCLE('',#7645,15.8113883008419);
#2937=CIRCLE('',#7646,17.0367250374008);
#2938=CIRCLE('',#7647,15.8113883008419);
#2939=CIRCLE('',#7668,1.5);
#2940=CIRCLE('',#7669,1.5);
#2941=CIRCLE('',#7671,1.65);
#2942=CIRCLE('',#7673,1.65);
#2943=CIRCLE('',#7675,13.819985714474);
#2944=CIRCLE('',#7677,21.9689920245294);
#2945=CIRCLE('',#7678,21.9689920245294);
#2946=CIRCLE('',#7680,21.9689920245294);
#2947=CIRCLE('',#7681,21.9689920245294);
#2948=CIRCLE('',#7683,13.819985714474);
#2949=CIRCLE('',#7684,14.0321508983363);
#2950=CIRCLE('',#7685,14.0321508983363);
#2951=CIRCLE('',#7689,19.25);
#2952=CIRCLE('',#7690,19.25);
#2953=CIRCLE('',#7702,1.5);
#2954=CIRCLE('',#7704,1.5);
#2955=CIRCLE('',#7712,1.1);
#2956=CIRCLE('',#7713,1.1);
#2957=CIRCLE('',#7715,1.1);
#2958=CIRCLE('',#7716,1.1);
#2959=CIRCLE('',#7718,1.1);
#2960=CIRCLE('',#7719,1.1);
#2961=CIRCLE('',#7721,13.819985714474);
#2962=CIRCLE('',#7722,14.1700407574314);
#2963=CIRCLE('',#7725,1.1);
#2964=CIRCLE('',#7727,1.1);
#2965=CIRCLE('',#7730,14.2852441859577);
#2966=CIRCLE('',#7732,19.25);
#2967=CIRCLE('',#7733,13.243680107935);
#2968=CIRCLE('',#7734,19.25);
#2969=CIRCLE('',#7738,35.0622035609646);
#2970=CIRCLE('',#7739,10.);
#2971=CIRCLE('',#7741,10.);
#2972=CIRCLE('',#7742,35.0622035609646);
#2973=CIRCLE('',#7745,14.2852441859577);
#2974=CIRCLE('',#7747,1.1);
#2975=CIRCLE('',#7748,1.1);
#2976=CIRCLE('',#7751,1.1);
#2977=CIRCLE('',#7752,1.1);
#2978=CIRCLE('',#7759,1.1);
#2979=CIRCLE('',#7760,1.1);
#2980=CIRCLE('',#7762,1.1);
#2981=CIRCLE('',#7763,1.1);
#2982=CIRCLE('',#7777,10.8559587775082);
#2983=CIRCLE('',#7778,13.5301235990631);
#2984=CIRCLE('',#7779,13.82);
#2985=CIRCLE('',#7780,46.3311569126792);
#2986=CIRCLE('',#7785,2.);
#2987=CIRCLE('',#7786,2.);
#2988=CIRCLE('',#7788,1.2);
#2989=CIRCLE('',#7789,1.2);
#2990=CIRCLE('',#7791,3.2);
#2991=CIRCLE('',#7792,3.2);
#2992=CIRCLE('',#7796,2.4);
#2993=CIRCLE('',#7799,2.4);
#2994=CIRCLE('',#7805,0.799999999999998);
#2995=CIRCLE('',#7806,0.799999999999998);
#2996=CIRCLE('',#7808,1.6);
#2997=CIRCLE('',#7809,1.6);
#2998=CIRCLE('',#7811,2.);
#2999=CIRCLE('',#7812,2.);
#3000=VERTEX_POINT('',#9888);
#3001=VERTEX_POINT('',#9889);
#3002=VERTEX_POINT('',#9891);
#3003=VERTEX_POINT('',#9893);
#3004=VERTEX_POINT('',#9897);
#3005=VERTEX_POINT('',#9898);
#3006=VERTEX_POINT('',#9900);
#3007=VERTEX_POINT('',#9902);
#3008=VERTEX_POINT('',#9906);
#3009=VERTEX_POINT('',#9907);
#3010=VERTEX_POINT('',#9909);
#3011=VERTEX_POINT('',#9913);
#3012=VERTEX_POINT('',#9915);
#3013=VERTEX_POINT('',#9919);
#3014=VERTEX_POINT('',#9921);
#3015=VERTEX_POINT('',#9925);
#3016=VERTEX_POINT('',#9927);
#3017=VERTEX_POINT('',#9932);
#3018=VERTEX_POINT('',#9933);
#3019=VERTEX_POINT('',#9935);
#3020=VERTEX_POINT('',#9937);
#3021=VERTEX_POINT('',#9941);
#3022=VERTEX_POINT('',#9942);
#3023=VERTEX_POINT('',#9944);
#3024=VERTEX_POINT('',#9946);
#3025=VERTEX_POINT('',#9948);
#3026=VERTEX_POINT('',#9950);
#3027=VERTEX_POINT('',#9955);
#3028=VERTEX_POINT('',#9956);
#3029=VERTEX_POINT('',#9961);
#3030=VERTEX_POINT('',#9962);
#3031=VERTEX_POINT('',#9966);
#3032=VERTEX_POINT('',#9968);
#3033=VERTEX_POINT('',#9972);
#3034=VERTEX_POINT('',#9973);
#3035=VERTEX_POINT('',#9976);
#3036=VERTEX_POINT('',#9979);
#3037=VERTEX_POINT('',#9980);
#3038=VERTEX_POINT('',#9982);
#3039=VERTEX_POINT('',#9984);
#3040=VERTEX_POINT('',#9988);
#3041=VERTEX_POINT('',#9989);
#3042=VERTEX_POINT('',#9991);
#3043=VERTEX_POINT('',#9993);
#3044=VERTEX_POINT('',#9999);
#3045=VERTEX_POINT('',#10000);
#3046=VERTEX_POINT('',#10002);
#3047=VERTEX_POINT('',#10004);
#3048=VERTEX_POINT('',#10008);
#3049=VERTEX_POINT('',#10009);
#3050=VERTEX_POINT('',#10011);
#3051=VERTEX_POINT('',#10013);
#3052=VERTEX_POINT('',#10017);
#3053=VERTEX_POINT('',#10018);
#3054=VERTEX_POINT('',#10020);
#3055=VERTEX_POINT('',#10022);
#3056=VERTEX_POINT('',#10026);
#3057=VERTEX_POINT('',#10027);
#3058=VERTEX_POINT('',#10029);
#3059=VERTEX_POINT('',#10034);
#3060=VERTEX_POINT('',#10035);
#3061=VERTEX_POINT('',#10038);
#3062=VERTEX_POINT('',#10040);
#3063=VERTEX_POINT('',#10042);
#3064=VERTEX_POINT('',#10044);
#3065=VERTEX_POINT('',#10048);
#3066=VERTEX_POINT('',#10050);
#3067=VERTEX_POINT('',#10053);
#3068=VERTEX_POINT('',#10055);
#3069=VERTEX_POINT('',#10057);
#3070=VERTEX_POINT('',#10061);
#3071=VERTEX_POINT('',#10063);
#3072=VERTEX_POINT('',#10066);
#3073=VERTEX_POINT('',#10070);
#3074=VERTEX_POINT('',#10072);
#3075=VERTEX_POINT('',#10075);
#3076=VERTEX_POINT('',#10158);
#3077=VERTEX_POINT('',#10159);
#3078=VERTEX_POINT('',#10178);
#3079=VERTEX_POINT('',#10180);
#3080=VERTEX_POINT('',#10182);
#3081=VERTEX_POINT('',#10184);
#3082=VERTEX_POINT('',#10186);
#3083=VERTEX_POINT('',#10188);
#3084=VERTEX_POINT('',#10190);
#3085=VERTEX_POINT('',#10192);
#3086=VERTEX_POINT('',#10196);
#3087=VERTEX_POINT('',#10198);
#3088=VERTEX_POINT('',#10202);
#3089=VERTEX_POINT('',#10204);
#3090=VERTEX_POINT('',#10208);
#3091=VERTEX_POINT('',#10210);
#3092=VERTEX_POINT('',#10214);
#3093=VERTEX_POINT('',#10216);
#3094=VERTEX_POINT('',#10220);
#3095=VERTEX_POINT('',#10222);
#3096=VERTEX_POINT('',#10224);
#3097=VERTEX_POINT('',#10263);
#3098=VERTEX_POINT('',#10264);
#3099=VERTEX_POINT('',#10283);
#3100=VERTEX_POINT('',#10306);
#3101=VERTEX_POINT('',#10307);
#3102=VERTEX_POINT('',#10309);
#3103=VERTEX_POINT('',#10314);
#3104=VERTEX_POINT('',#10333);
#3105=VERTEX_POINT('',#10341);
#3106=VERTEX_POINT('',#10343);
#3107=VERTEX_POINT('',#10345);
#3108=VERTEX_POINT('',#10398);
#3109=VERTEX_POINT('',#10400);
#3110=VERTEX_POINT('',#10408);
#3111=VERTEX_POINT('',#10432);
#3112=VERTEX_POINT('',#10436);
#3113=VERTEX_POINT('',#10440);
#3114=VERTEX_POINT('',#10442);
#3115=VERTEX_POINT('',#10446);
#3116=VERTEX_POINT('',#10447);
#3117=VERTEX_POINT('',#10449);
#3118=VERTEX_POINT('',#10451);
#3119=VERTEX_POINT('',#10467);
#3120=VERTEX_POINT('',#10468);
#3121=VERTEX_POINT('',#10473);
#3122=VERTEX_POINT('',#10474);
#3123=VERTEX_POINT('',#10476);
#3124=VERTEX_POINT('',#10478);
#3125=VERTEX_POINT('',#10482);
#3126=VERTEX_POINT('',#10484);
#3127=VERTEX_POINT('',#10493);
#3128=VERTEX_POINT('',#10495);
#3129=VERTEX_POINT('',#10499);
#3130=VERTEX_POINT('',#10500);
#3131=VERTEX_POINT('',#10502);
#3132=VERTEX_POINT('',#10504);
#3133=VERTEX_POINT('',#10507);
#3134=VERTEX_POINT('',#10511);
#3135=VERTEX_POINT('',#10515);
#3136=VERTEX_POINT('',#10518);
#3137=VERTEX_POINT('',#10522);
#3138=VERTEX_POINT('',#10525);
#3139=VERTEX_POINT('',#10530);
#3140=VERTEX_POINT('',#10532);
#3141=VERTEX_POINT('',#10537);
#3142=VERTEX_POINT('',#10538);
#3143=VERTEX_POINT('',#10558);
#3144=VERTEX_POINT('',#10559);
#3145=VERTEX_POINT('',#10561);
#3146=VERTEX_POINT('',#10563);
#3147=VERTEX_POINT('',#10567);
#3148=VERTEX_POINT('',#10570);
#3149=VERTEX_POINT('',#10574);
#3150=VERTEX_POINT('',#10579);
#3151=VERTEX_POINT('',#10588);
#3152=VERTEX_POINT('',#10590);
#3153=VERTEX_POINT('',#10594);
#3154=VERTEX_POINT('',#10596);
#3155=VERTEX_POINT('',#10600);
#3156=VERTEX_POINT('',#10602);
#3157=VERTEX_POINT('',#10606);
#3158=VERTEX_POINT('',#10608);
#3159=VERTEX_POINT('',#10612);
#3160=VERTEX_POINT('',#10614);
#3161=VERTEX_POINT('',#10616);
#3162=VERTEX_POINT('',#10655);
#3163=VERTEX_POINT('',#10656);
#3164=VERTEX_POINT('',#10675);
#3165=VERTEX_POINT('',#10698);
#3166=VERTEX_POINT('',#10699);
#3167=VERTEX_POINT('',#10701);
#3168=VERTEX_POINT('',#10706);
#3169=VERTEX_POINT('',#10717);
#3170=VERTEX_POINT('',#10728);
#3171=VERTEX_POINT('',#10739);
#3172=VERTEX_POINT('',#10747);
#3173=VERTEX_POINT('',#10749);
#3174=VERTEX_POINT('',#10751);
#3175=VERTEX_POINT('',#10796);
#3176=VERTEX_POINT('',#10798);
#3177=VERTEX_POINT('',#10806);
#3178=VERTEX_POINT('',#10817);
#3179=VERTEX_POINT('',#10828);
#3180=VERTEX_POINT('',#10844);
#3181=VERTEX_POINT('',#10845);
#3182=VERTEX_POINT('',#10858);
#3183=VERTEX_POINT('',#10860);
#3184=VERTEX_POINT('',#10864);
#3185=VERTEX_POINT('',#10865);
#3186=VERTEX_POINT('',#10867);
#3187=VERTEX_POINT('',#10869);
#3188=VERTEX_POINT('',#10875);
#3189=VERTEX_POINT('',#10876);
#3190=VERTEX_POINT('',#10878);
#3191=VERTEX_POINT('',#10880);
#3192=VERTEX_POINT('',#10884);
#3193=VERTEX_POINT('',#10885);
#3194=VERTEX_POINT('',#10887);
#3195=VERTEX_POINT('',#10889);
#3196=VERTEX_POINT('',#10893);
#3197=VERTEX_POINT('',#10911);
#3198=VERTEX_POINT('',#10930);
#3199=VERTEX_POINT('',#10932);
#3200=VERTEX_POINT('',#10936);
#3201=VERTEX_POINT('',#10937);
#3202=VERTEX_POINT('',#10939);
#3203=VERTEX_POINT('',#10941);
#3204=VERTEX_POINT('',#10944);
#3205=VERTEX_POINT('',#10948);
#3206=VERTEX_POINT('',#10952);
#3207=VERTEX_POINT('',#10955);
#3208=VERTEX_POINT('',#10959);
#3209=VERTEX_POINT('',#10961);
#3210=VERTEX_POINT('',#10963);
#3211=VERTEX_POINT('',#10965);
#3212=VERTEX_POINT('',#10969);
#3213=VERTEX_POINT('',#10970);
#3214=VERTEX_POINT('',#10972);
#3215=VERTEX_POINT('',#10974);
#3216=VERTEX_POINT('',#10979);
#3217=VERTEX_POINT('',#10980);
#3218=VERTEX_POINT('',#10985);
#3219=VERTEX_POINT('',#10986);
#3220=VERTEX_POINT('',#10988);
#3221=VERTEX_POINT('',#10990);
#3222=VERTEX_POINT('',#11012);
#3223=VERTEX_POINT('',#11013);
#3224=VERTEX_POINT('',#11015);
#3225=VERTEX_POINT('',#11017);
#3226=VERTEX_POINT('',#11021);
#3227=VERTEX_POINT('',#11024);
#3228=VERTEX_POINT('',#11028);
#3229=VERTEX_POINT('',#11033);
#3230=VERTEX_POINT('',#11049);
#3231=VERTEX_POINT('',#11051);
#3232=VERTEX_POINT('',#11055);
#3233=VERTEX_POINT('',#11057);
#3234=VERTEX_POINT('',#11061);
#3235=VERTEX_POINT('',#11063);
#3236=VERTEX_POINT('',#11067);
#3237=VERTEX_POINT('',#11069);
#3238=VERTEX_POINT('',#11073);
#3239=VERTEX_POINT('',#11075);
#3240=VERTEX_POINT('',#11077);
#3241=VERTEX_POINT('',#11116);
#3242=VERTEX_POINT('',#11117);
#3243=VERTEX_POINT('',#11136);
#3244=VERTEX_POINT('',#11159);
#3245=VERTEX_POINT('',#11160);
#3246=VERTEX_POINT('',#11162);
#3247=VERTEX_POINT('',#11167);
#3248=VERTEX_POINT('',#11176);
#3249=VERTEX_POINT('',#11181);
#3250=VERTEX_POINT('',#11188);
#3251=VERTEX_POINT('',#11199);
#3252=VERTEX_POINT('',#11210);
#3253=VERTEX_POINT('',#11218);
#3254=VERTEX_POINT('',#11220);
#3255=VERTEX_POINT('',#11222);
#3256=VERTEX_POINT('',#11259);
#3257=VERTEX_POINT('',#11261);
#3258=VERTEX_POINT('',#11269);
#3259=VERTEX_POINT('',#11280);
#3260=VERTEX_POINT('',#11291);
#3261=VERTEX_POINT('',#11298);
#3262=VERTEX_POINT('',#11303);
#3263=VERTEX_POINT('',#11317);
#3264=VERTEX_POINT('',#11319);
#3265=VERTEX_POINT('',#11323);
#3266=VERTEX_POINT('',#11324);
#3267=VERTEX_POINT('',#11329);
#3268=VERTEX_POINT('',#11330);
#3269=VERTEX_POINT('',#11358);
#3270=VERTEX_POINT('',#11412);
#3271=VERTEX_POINT('',#11413);
#3272=VERTEX_POINT('',#11422);
#3273=VERTEX_POINT('',#11424);
#3274=VERTEX_POINT('',#11428);
#3275=VERTEX_POINT('',#11429);
#3276=VERTEX_POINT('',#11431);
#3277=VERTEX_POINT('',#11433);
#3278=VERTEX_POINT('',#11439);
#3279=VERTEX_POINT('',#11440);
#3280=VERTEX_POINT('',#11442);
#3281=VERTEX_POINT('',#11444);
#3282=VERTEX_POINT('',#11448);
#3283=VERTEX_POINT('',#11450);
#3284=VERTEX_POINT('',#11454);
#3285=VERTEX_POINT('',#11460);
#3286=VERTEX_POINT('',#11467);
#3287=VERTEX_POINT('',#11469);
#3288=VERTEX_POINT('',#11473);
#3289=VERTEX_POINT('',#11474);
#3290=VERTEX_POINT('',#11476);
#3291=VERTEX_POINT('',#11478);
#3292=VERTEX_POINT('',#11481);
#3293=VERTEX_POINT('',#11485);
#3294=VERTEX_POINT('',#11489);
#3295=VERTEX_POINT('',#11492);
#3296=VERTEX_POINT('',#11496);
#3297=VERTEX_POINT('',#11498);
#3298=VERTEX_POINT('',#11500);
#3299=VERTEX_POINT('',#11502);
#3300=VERTEX_POINT('',#11506);
#3301=VERTEX_POINT('',#11507);
#3302=VERTEX_POINT('',#11509);
#3303=VERTEX_POINT('',#11511);
#3304=VERTEX_POINT('',#11516);
#3305=VERTEX_POINT('',#11517);
#3306=VERTEX_POINT('',#11522);
#3307=VERTEX_POINT('',#11523);
#3308=VERTEX_POINT('',#11525);
#3309=VERTEX_POINT('',#11527);
#3310=VERTEX_POINT('',#11549);
#3311=VERTEX_POINT('',#11550);
#3312=VERTEX_POINT('',#11552);
#3313=VERTEX_POINT('',#11554);
#3314=VERTEX_POINT('',#11558);
#3315=VERTEX_POINT('',#11561);
#3316=VERTEX_POINT('',#11565);
#3317=VERTEX_POINT('',#11570);
#3318=VERTEX_POINT('',#11589);
#3319=VERTEX_POINT('',#11591);
#3320=VERTEX_POINT('',#11595);
#3321=VERTEX_POINT('',#11597);
#3322=VERTEX_POINT('',#11601);
#3323=VERTEX_POINT('',#11603);
#3324=VERTEX_POINT('',#11607);
#3325=VERTEX_POINT('',#11608);
#3326=VERTEX_POINT('',#11610);
#3327=VERTEX_POINT('',#11612);
#3328=VERTEX_POINT('',#11617);
#3329=VERTEX_POINT('',#11618);
#3330=VERTEX_POINT('',#11623);
#3331=VERTEX_POINT('',#11627);
#3332=VERTEX_POINT('',#11636);
#3333=VERTEX_POINT('',#11638);
#3334=VERTEX_POINT('',#11642);
#3335=VERTEX_POINT('',#11643);
#3336=VERTEX_POINT('',#11645);
#3337=VERTEX_POINT('',#11647);
#3338=VERTEX_POINT('',#11651);
#3339=VERTEX_POINT('',#11653);
#3340=VERTEX_POINT('',#11657);
#3341=VERTEX_POINT('',#11658);
#3342=VERTEX_POINT('',#11660);
#3343=VERTEX_POINT('',#11662);
#3344=VERTEX_POINT('',#11679);
#3345=VERTEX_POINT('',#11681);
#3346=VERTEX_POINT('',#11685);
#3347=VERTEX_POINT('',#11687);
#3348=VERTEX_POINT('',#11691);
#3349=VERTEX_POINT('',#11693);
#3350=VERTEX_POINT('',#11697);
#3351=VERTEX_POINT('',#11698);
#3352=VERTEX_POINT('',#11700);
#3353=VERTEX_POINT('',#11702);
#3354=VERTEX_POINT('',#11707);
#3355=VERTEX_POINT('',#11708);
#3356=VERTEX_POINT('',#11713);
#3357=VERTEX_POINT('',#11717);
#3358=VERTEX_POINT('',#11726);
#3359=VERTEX_POINT('',#11728);
#3360=VERTEX_POINT('',#11732);
#3361=VERTEX_POINT('',#11733);
#3362=VERTEX_POINT('',#11735);
#3363=VERTEX_POINT('',#11737);
#3364=VERTEX_POINT('',#11741);
#3365=VERTEX_POINT('',#11743);
#3366=VERTEX_POINT('',#11747);
#3367=VERTEX_POINT('',#11748);
#3368=VERTEX_POINT('',#11750);
#3369=VERTEX_POINT('',#11752);
#3370=VERTEX_POINT('',#11769);
#3371=VERTEX_POINT('',#11771);
#3372=VERTEX_POINT('',#11775);
#3373=VERTEX_POINT('',#11777);
#3374=VERTEX_POINT('',#11781);
#3375=VERTEX_POINT('',#11783);
#3376=VERTEX_POINT('',#11787);
#3377=VERTEX_POINT('',#11788);
#3378=VERTEX_POINT('',#11790);
#3379=VERTEX_POINT('',#11792);
#3380=VERTEX_POINT('',#11797);
#3381=VERTEX_POINT('',#11798);
#3382=VERTEX_POINT('',#11803);
#3383=VERTEX_POINT('',#11807);
#3384=VERTEX_POINT('',#11816);
#3385=VERTEX_POINT('',#11818);
#3386=VERTEX_POINT('',#11822);
#3387=VERTEX_POINT('',#11823);
#3388=VERTEX_POINT('',#11825);
#3389=VERTEX_POINT('',#11827);
#3390=VERTEX_POINT('',#11831);
#3391=VERTEX_POINT('',#11833);
#3392=VERTEX_POINT('',#11837);
#3393=VERTEX_POINT('',#11838);
#3394=VERTEX_POINT('',#11840);
#3395=VERTEX_POINT('',#11842);
#3396=VERTEX_POINT('',#11856);
#3397=VERTEX_POINT('',#11858);
#3398=VERTEX_POINT('',#11862);
#3399=VERTEX_POINT('',#11864);
#3400=VERTEX_POINT('',#11868);
#3401=VERTEX_POINT('',#11870);
#3402=VERTEX_POINT('',#11874);
#3403=VERTEX_POINT('',#11875);
#3404=VERTEX_POINT('',#11877);
#3405=VERTEX_POINT('',#11879);
#3406=VERTEX_POINT('',#11883);
#3407=VERTEX_POINT('',#11884);
#3408=VERTEX_POINT('',#11886);
#3409=VERTEX_POINT('',#11889);
#3410=VERTEX_POINT('',#11893);
#3411=VERTEX_POINT('',#11895);
#3412=VERTEX_POINT('',#11899);
#3413=VERTEX_POINT('',#11901);
#3414=VERTEX_POINT('',#11903);
#3415=VERTEX_POINT('',#11905);
#3416=VERTEX_POINT('',#11913);
#3417=VERTEX_POINT('',#11915);
#3418=VERTEX_POINT('',#11917);
#3419=VERTEX_POINT('',#11921);
#3420=VERTEX_POINT('',#11922);
#3421=VERTEX_POINT('',#11925);
#3422=VERTEX_POINT('',#11942);
#3423=VERTEX_POINT('',#11944);
#3424=VERTEX_POINT('',#11946);
#3425=VERTEX_POINT('',#11991);
#3426=VERTEX_POINT('',#11992);
#3427=VERTEX_POINT('',#12016);
#3428=VERTEX_POINT('',#12066);
#3429=VERTEX_POINT('',#12068);
#3430=VERTEX_POINT('',#12097);
#3431=VERTEX_POINT('',#12143);
#3432=VERTEX_POINT('',#12144);
#3433=VERTEX_POINT('',#12146);
#3434=VERTEX_POINT('',#12148);
#3435=VERTEX_POINT('',#12152);
#3436=VERTEX_POINT('',#12153);
#3437=VERTEX_POINT('',#12155);
#3438=VERTEX_POINT('',#12157);
#3439=VERTEX_POINT('',#12178);
#3440=VERTEX_POINT('',#12180);
#3441=VERTEX_POINT('',#12184);
#3442=VERTEX_POINT('',#12186);
#3443=VERTEX_POINT('',#12190);
#3444=VERTEX_POINT('',#12192);
#3445=VERTEX_POINT('',#12196);
#3446=VERTEX_POINT('',#12198);
#3447=VERTEX_POINT('',#12202);
#3448=VERTEX_POINT('',#12204);
#3449=VERTEX_POINT('',#12206);
#3450=VERTEX_POINT('',#12208);
#3451=VERTEX_POINT('',#12211);
#3452=VERTEX_POINT('',#12213);
#3453=VERTEX_POINT('',#12216);
#3454=VERTEX_POINT('',#12217);
#3455=VERTEX_POINT('',#12219);
#3456=VERTEX_POINT('',#12221);
#3457=VERTEX_POINT('',#12224);
#3458=VERTEX_POINT('',#12225);
#3459=VERTEX_POINT('',#12227);
#3460=VERTEX_POINT('',#12229);
#3461=VERTEX_POINT('',#12233);
#3462=VERTEX_POINT('',#12234);
#3463=VERTEX_POINT('',#12236);
#3464=VERTEX_POINT('',#12238);
#3465=VERTEX_POINT('',#12242);
#3466=VERTEX_POINT('',#12244);
#3467=VERTEX_POINT('',#12248);
#3468=VERTEX_POINT('',#12252);
#3469=VERTEX_POINT('',#12259);
#3470=VERTEX_POINT('',#12263);
#3471=VERTEX_POINT('',#12270);
#3472=VERTEX_POINT('',#12271);
#3473=VERTEX_POINT('',#12275);
#3474=VERTEX_POINT('',#12277);
#3475=VERTEX_POINT('',#12281);
#3476=VERTEX_POINT('',#12285);
#3477=VERTEX_POINT('',#12287);
#3478=VERTEX_POINT('',#12289);
#3479=VERTEX_POINT('',#12303);
#3480=VERTEX_POINT('',#12305);
#3481=VERTEX_POINT('',#12309);
#3482=VERTEX_POINT('',#12311);
#3483=VERTEX_POINT('',#12313);
#3484=VERTEX_POINT('',#12352);
#3485=VERTEX_POINT('',#12353);
#3486=VERTEX_POINT('',#12372);
#3487=VERTEX_POINT('',#12395);
#3488=VERTEX_POINT('',#12396);
#3489=VERTEX_POINT('',#12398);
#3490=VERTEX_POINT('',#12400);
#3491=VERTEX_POINT('',#12404);
#3492=VERTEX_POINT('',#12405);
#3493=VERTEX_POINT('',#12408);
#3494=VERTEX_POINT('',#12423);
#3495=VERTEX_POINT('',#12425);
#3496=VERTEX_POINT('',#12440);
#3497=VERTEX_POINT('',#12444);
#3498=VERTEX_POINT('',#12446);
#3499=VERTEX_POINT('',#12448);
#3500=VERTEX_POINT('',#12450);
#3501=VERTEX_POINT('',#12480);
#3502=VERTEX_POINT('',#12484);
#3503=VERTEX_POINT('',#12486);
#3504=VERTEX_POINT('',#12494);
#3505=VERTEX_POINT('',#12537);
#3506=VERTEX_POINT('',#12545);
#3507=VERTEX_POINT('',#12555);
#3508=VERTEX_POINT('',#12556);
#3509=VERTEX_POINT('',#12561);
#3510=VERTEX_POINT('',#12565);
#3511=VERTEX_POINT('',#12572);
#3512=VERTEX_POINT('',#12574);
#3513=VERTEX_POINT('',#12578);
#3514=VERTEX_POINT('',#12580);
#3515=VERTEX_POINT('',#12590);
#3516=VERTEX_POINT('',#12592);
#3517=VERTEX_POINT('',#12594);
#3518=VERTEX_POINT('',#12637);
#3519=VERTEX_POINT('',#12638);
#3520=VERTEX_POINT('',#12659);
#3521=VERTEX_POINT('',#12684);
#3522=VERTEX_POINT('',#12685);
#3523=VERTEX_POINT('',#12704);
#3524=VERTEX_POINT('',#12706);
#3525=VERTEX_POINT('',#12708);
#3526=VERTEX_POINT('',#12710);
#3527=VERTEX_POINT('',#12712);
#3528=VERTEX_POINT('',#12714);
#3529=VERTEX_POINT('',#12716);
#3530=VERTEX_POINT('',#12718);
#3531=VERTEX_POINT('',#12722);
#3532=VERTEX_POINT('',#12724);
#3533=VERTEX_POINT('',#12728);
#3534=VERTEX_POINT('',#12730);
#3535=VERTEX_POINT('',#12734);
#3536=VERTEX_POINT('',#12736);
#3537=VERTEX_POINT('',#12740);
#3538=VERTEX_POINT('',#12741);
#3539=VERTEX_POINT('',#12752);
#3540=VERTEX_POINT('',#12763);
#3541=VERTEX_POINT('',#12778);
#3542=VERTEX_POINT('',#12782);
#3543=VERTEX_POINT('',#12784);
#3544=VERTEX_POINT('',#12788);
#3545=VERTEX_POINT('',#12803);
#3546=VERTEX_POINT('',#12814);
#3547=VERTEX_POINT('',#12825);
#3548=VERTEX_POINT('',#12829);
#3549=VERTEX_POINT('',#12837);
#3550=VERTEX_POINT('',#12841);
#3551=VERTEX_POINT('',#12845);
#3552=VERTEX_POINT('',#12847);
#3553=VERTEX_POINT('',#12851);
#3554=VERTEX_POINT('',#12852);
#3555=VERTEX_POINT('',#12854);
#3556=VERTEX_POINT('',#12856);
#3557=VERTEX_POINT('',#12860);
#3558=VERTEX_POINT('',#12873);
#3559=VERTEX_POINT('',#12874);
#3560=VERTEX_POINT('',#12878);
#3561=VERTEX_POINT('',#12880);
#3562=VERTEX_POINT('',#12888);
#3563=VERTEX_POINT('',#12889);
#3564=VERTEX_POINT('',#12892);
#3565=VERTEX_POINT('',#12894);
#3566=VERTEX_POINT('',#12898);
#3567=VERTEX_POINT('',#12900);
#3568=VERTEX_POINT('',#12902);
#3569=VERTEX_POINT('',#12904);
#3570=VERTEX_POINT('',#12910);
#3571=VERTEX_POINT('',#12912);
#3572=VERTEX_POINT('',#12914);
#3573=VERTEX_POINT('',#12918);
#3574=VERTEX_POINT('',#12919);
#3575=VERTEX_POINT('',#12921);
#3576=VERTEX_POINT('',#12923);
#3577=VERTEX_POINT('',#12926);
#3578=VERTEX_POINT('',#12930);
#3579=VERTEX_POINT('',#12934);
#3580=VERTEX_POINT('',#12937);
#3581=VERTEX_POINT('',#12943);
#3582=VERTEX_POINT('',#12946);
#3583=VERTEX_POINT('',#12951);
#3584=VERTEX_POINT('',#12953);
#3585=VERTEX_POINT('',#12958);
#3586=VERTEX_POINT('',#12959);
#3587=VERTEX_POINT('',#13015);
#3588=VERTEX_POINT('',#13017);
#3589=VERTEX_POINT('',#13046);
#3590=VERTEX_POINT('',#13053);
#3591=VERTEX_POINT('',#13055);
#3592=VERTEX_POINT('',#13059);
#3593=VERTEX_POINT('',#13061);
#3594=VERTEX_POINT('',#13065);
#3595=VERTEX_POINT('',#13067);
#3596=VERTEX_POINT('',#13071);
#3597=VERTEX_POINT('',#13072);
#3598=VERTEX_POINT('',#13074);
#3599=VERTEX_POINT('',#13076);
#3600=VERTEX_POINT('',#13081);
#3601=VERTEX_POINT('',#13082);
#3602=VERTEX_POINT('',#13087);
#3603=VERTEX_POINT('',#13091);
#3604=VERTEX_POINT('',#13100);
#3605=VERTEX_POINT('',#13102);
#3606=VERTEX_POINT('',#13106);
#3607=VERTEX_POINT('',#13107);
#3608=VERTEX_POINT('',#13109);
#3609=VERTEX_POINT('',#13111);
#3610=VERTEX_POINT('',#13115);
#3611=VERTEX_POINT('',#13117);
#3612=VERTEX_POINT('',#13121);
#3613=VERTEX_POINT('',#13122);
#3614=VERTEX_POINT('',#13124);
#3615=VERTEX_POINT('',#13126);
#3616=EDGE_CURVE('',#3000,#3001,#2681,.T.);
#3617=EDGE_CURVE('',#3002,#3000,#2682,.T.);
#3618=EDGE_CURVE('',#3003,#3002,#2683,.T.);
#3619=EDGE_CURVE('',#3003,#3001,#2684,.T.);
#3620=EDGE_CURVE('',#3004,#3005,#2685,.T.);
#3621=EDGE_CURVE('',#3006,#3004,#2686,.T.);
#3622=EDGE_CURVE('',#3007,#3006,#2687,.T.);
#3623=EDGE_CURVE('',#3005,#3007,#2688,.T.);
#3624=EDGE_CURVE('',#3008,#3009,#2689,.T.);
#3625=EDGE_CURVE('',#3008,#3010,#2690,.T.);
#3626=EDGE_CURVE('',#3009,#3010,#2691,.T.);
#3627=EDGE_CURVE('',#3011,#3011,#2692,.T.);
#3628=EDGE_CURVE('',#3011,#3012,#610,.T.);
#3629=EDGE_CURVE('',#3012,#3012,#2693,.T.);
#3630=EDGE_CURVE('',#3013,#3013,#2694,.T.);
#3631=EDGE_CURVE('',#3013,#3014,#611,.T.);
#3632=EDGE_CURVE('',#3014,#3014,#2695,.T.);
#3633=EDGE_CURVE('',#3002,#3015,#2696,.T.);
#3634=EDGE_CURVE('',#3015,#3016,#612,.T.);
#3635=EDGE_CURVE('',#3016,#3004,#2697,.T.);
#3636=EDGE_CURVE('',#3002,#3004,#613,.T.);
#3637=EDGE_CURVE('',#3017,#3018,#614,.T.);
#3638=EDGE_CURVE('',#3017,#3019,#615,.T.);
#3639=EDGE_CURVE('',#3019,#3020,#616,.T.);
#3640=EDGE_CURVE('',#3018,#3020,#383,.T.);
#3641=EDGE_CURVE('',#3021,#3022,#617,.T.);
#3642=EDGE_CURVE('',#3021,#3023,#2698,.T.);
#3643=EDGE_CURVE('',#3023,#3024,#618,.T.);
#3644=EDGE_CURVE('',#3024,#3025,#2699,.T.);
#3645=EDGE_CURVE('',#3025,#3026,#619,.T.);
#3646=EDGE_CURVE('',#3026,#3017,#2700,.T.);
#3647=EDGE_CURVE('',#3022,#3018,#384,.T.);
#3648=EDGE_CURVE('',#3027,#3028,#620,.T.);
#3649=EDGE_CURVE('',#3027,#3021,#621,.T.);
#3650=EDGE_CURVE('',#3028,#3022,#385,.T.);
#3651=EDGE_CURVE('',#3029,#3030,#622,.T.);
#3652=EDGE_CURVE('',#3029,#3027,#2701,.T.);
#3653=EDGE_CURVE('',#3020,#3028,#386,.T.);
#3654=EDGE_CURVE('',#3019,#3031,#2702,.T.);
#3655=EDGE_CURVE('',#3032,#3031,#623,.T.);
#3656=EDGE_CURVE('',#3030,#3032,#2703,.T.);
#3657=EDGE_CURVE('',#3033,#3034,#2704,.T.);
#3658=EDGE_CURVE('',#3034,#3009,#624,.T.);
#3659=EDGE_CURVE('',#3009,#3035,#2705,.T.);
#3660=EDGE_CURVE('',#3035,#3033,#625,.T.);
#3661=EDGE_CURVE('',#3036,#3037,#626,.T.);
#3662=EDGE_CURVE('',#3038,#3037,#2706,.T.);
#3663=EDGE_CURVE('',#3039,#3038,#627,.T.);
#3664=EDGE_CURVE('',#3036,#3039,#2707,.T.);
#3665=EDGE_CURVE('',#3040,#3041,#628,.T.);
#3666=EDGE_CURVE('',#3042,#3040,#629,.T.);
#3667=EDGE_CURVE('',#3042,#3043,#630,.T.);
#3668=EDGE_CURVE('',#3041,#3043,#631,.T.);
#3669=EDGE_CURVE('',#3005,#3003,#632,.T.);
#3670=EDGE_CURVE('',#3044,#3045,#633,.T.);
#3671=EDGE_CURVE('',#3045,#3046,#634,.T.);
#3672=EDGE_CURVE('',#3046,#3047,#635,.T.);
#3673=EDGE_CURVE('',#3047,#3044,#636,.T.);
#3674=EDGE_CURVE('',#3048,#3049,#637,.T.);
#3675=EDGE_CURVE('',#3049,#3050,#638,.T.);
#3676=EDGE_CURVE('',#3050,#3051,#639,.T.);
#3677=EDGE_CURVE('',#3051,#3048,#640,.T.);
#3678=EDGE_CURVE('',#3052,#3053,#641,.T.);
#3679=EDGE_CURVE('',#3053,#3054,#642,.T.);
#3680=EDGE_CURVE('',#3054,#3055,#643,.T.);
#3681=EDGE_CURVE('',#3055,#3052,#644,.T.);
#3682=EDGE_CURVE('',#3056,#3057,#645,.T.);
#3683=EDGE_CURVE('',#3057,#3058,#646,.T.);
#3684=EDGE_CURVE('',#3058,#3008,#647,.T.);
#3685=EDGE_CURVE('',#3008,#3056,#648,.T.);
#3686=EDGE_CURVE('',#3059,#3060,#2708,.T.);
#3687=EDGE_CURVE('',#3060,#3000,#2709,.T.);
#3688=EDGE_CURVE('',#3061,#3001,#2710,.T.);
#3689=EDGE_CURVE('',#3061,#3062,#649,.T.);
#3690=EDGE_CURVE('',#3062,#3063,#650,.T.);
#3691=EDGE_CURVE('',#3063,#3064,#651,.T.);
#3692=EDGE_CURVE('',#3064,#3059,#652,.T.);
#3693=EDGE_CURVE('',#3007,#3065,#2711,.T.);
#3694=EDGE_CURVE('',#3006,#3066,#2712,.T.);
#3695=EDGE_CURVE('',#3066,#3010,#2713,.T.);
#3696=EDGE_CURVE('',#3010,#3067,#653,.T.);
#3697=EDGE_CURVE('',#3067,#3068,#654,.T.);
#3698=EDGE_CURVE('',#3068,#3069,#655,.T.);
#3699=EDGE_CURVE('',#3069,#3065,#656,.T.);
#3700=EDGE_CURVE('',#3036,#3070,#657,.T.);
#3701=EDGE_CURVE('',#3070,#3071,#2714,.T.);
#3702=EDGE_CURVE('',#3071,#3043,#658,.T.);
#3703=EDGE_CURVE('',#3072,#3042,#659,.T.);
#3704=EDGE_CURVE('',#3037,#3072,#660,.T.);
#3705=EDGE_CURVE('',#3073,#3041,#661,.T.);
#3706=EDGE_CURVE('',#3073,#3074,#2715,.T.);
#3707=EDGE_CURVE('',#3039,#3074,#662,.T.);
#3708=EDGE_CURVE('',#3075,#3038,#663,.T.);
#3709=EDGE_CURVE('',#3075,#3040,#664,.T.);
#3710=EDGE_CURVE('',#3071,#3073,#665,.T.);
#3711=EDGE_CURVE('',#3074,#3070,#666,.T.);
#3712=EDGE_CURVE('',#3072,#3075,#667,.T.);
#3713=EDGE_CURVE('',#3068,#3054,#2716,.T.);
#3714=EDGE_CURVE('',#3055,#3067,#2717,.T.);
#3715=EDGE_CURVE('',#3068,#3051,#2718,.T.);
#3716=EDGE_CURVE('',#3051,#3054,#2719,.T.);
#3717=EDGE_CURVE('',#3055,#3058,#2720,.T.);
#3718=EDGE_CURVE('',#3058,#3067,#2721,.T.);
#3719=EDGE_CURVE('',#3048,#3053,#2722,.T.);
#3720=EDGE_CURVE('',#3069,#3050,#2723,.T.);
#3721=EDGE_CURVE('',#3052,#3057,#2724,.T.);
#3722=EDGE_CURVE('',#3053,#3063,#2725,.T.);
#3723=EDGE_CURVE('',#3064,#3052,#2726,.T.);
#3724=EDGE_CURVE('',#3048,#3063,#2727,.T.);
#3725=EDGE_CURVE('',#3069,#3047,#2728,.T.);
#3726=EDGE_CURVE('',#3047,#3050,#2729,.T.);
#3727=EDGE_CURVE('',#3064,#3057,#2730,.T.);
#3728=EDGE_CURVE('',#3049,#3062,#2731,.T.);
#3729=EDGE_CURVE('',#3044,#3049,#2732,.T.);
#3730=EDGE_CURVE('',#3065,#3046,#2733,.T.);
#3731=EDGE_CURVE('',#3066,#3016,#2734,.T.);
#3732=EDGE_CURVE('',#3035,#3066,#2735,.T.);
#3733=EDGE_CURVE('',#3056,#3034,#2736,.T.);
#3734=EDGE_CURVE('',#3059,#3056,#2737,.T.);
#3735=EDGE_CURVE('',#3044,#3062,#2738,.T.);
#3736=EDGE_CURVE('',#3005,#3046,#2739,.T.);
#3737=EDGE_CURVE('',#3035,#3016,#2740,.T.);
#3738=EDGE_CURVE('',#3059,#3034,#2741,.T.);
#3739=EDGE_CURVE('',#3045,#3061,#2742,.T.);
#3740=EDGE_CURVE('',#3003,#3045,#2743,.T.);
#3741=EDGE_CURVE('',#3033,#3015,#2744,.T.);
#3742=EDGE_CURVE('',#3060,#3033,#2745,.T.);
#3743=EDGE_CURVE('',#3060,#3015,#2746,.T.);
#3744=EDGE_CURVE('',#3032,#3025,#668,.T.);
#3745=EDGE_CURVE('',#3030,#3024,#669,.T.);
#3746=EDGE_CURVE('',#3031,#3026,#670,.T.);
#3747=EDGE_CURVE('',#3023,#3029,#671,.T.);
#3748=EDGE_CURVE('',#3076,#3077,#127,.T.);
#3749=EDGE_CURVE('',#3078,#3077,#387,.T.);
#3750=EDGE_CURVE('',#3079,#3078,#672,.T.);
#3751=EDGE_CURVE('',#3080,#3079,#388,.T.);
#3752=EDGE_CURVE('',#3080,#3081,#673,.T.);
#3753=EDGE_CURVE('',#3082,#3081,#389,.T.);
#3754=EDGE_CURVE('',#3083,#3082,#674,.T.);
#3755=EDGE_CURVE('',#3084,#3083,#390,.T.);
#3756=EDGE_CURVE('',#3085,#3084,#675,.T.);
#3757=EDGE_CURVE('',#3076,#3085,#391,.T.);
#3758=EDGE_CURVE('',#3086,#3086,#2747,.T.);
#3759=EDGE_CURVE('',#3086,#3087,#676,.T.);
#3760=EDGE_CURVE('',#3087,#3087,#2748,.T.);
#3761=EDGE_CURVE('',#3088,#3088,#2749,.T.);
#3762=EDGE_CURVE('',#3088,#3089,#677,.T.);
#3763=EDGE_CURVE('',#3089,#3089,#2750,.T.);
#3764=EDGE_CURVE('',#3090,#3090,#2751,.T.);
#3765=EDGE_CURVE('',#3090,#3091,#678,.T.);
#3766=EDGE_CURVE('',#3091,#3091,#2752,.T.);
#3767=EDGE_CURVE('',#3092,#3092,#2753,.T.);
#3768=EDGE_CURVE('',#3092,#3093,#679,.T.);
#3769=EDGE_CURVE('',#3093,#3093,#2754,.T.);
#3770=EDGE_CURVE('',#3094,#3094,#2755,.T.);
#3771=EDGE_CURVE('',#3094,#3095,#680,.T.);
#3772=EDGE_CURVE('',#3095,#3096,#128,.T.);
#3773=EDGE_CURVE('',#3096,#3095,#129,.T.);
#3774=EDGE_CURVE('',#3097,#3098,#130,.T.);
#3775=EDGE_CURVE('',#3098,#3099,#681,.T.);
#3776=EDGE_CURVE('',#3099,#3099,#2756,.T.);
#3777=EDGE_CURVE('',#3098,#3097,#131,.T.);
#3778=EDGE_CURVE('',#3100,#3101,#2757,.T.);
#3779=EDGE_CURVE('',#3102,#3100,#132,.T.);
#3780=EDGE_CURVE('',#3103,#3102,#133,.T.);
#3781=EDGE_CURVE('',#3103,#3104,#134,.T.);
#3782=EDGE_CURVE('',#3104,#3105,#2758,.T.);
#3783=EDGE_CURVE('',#3105,#3106,#682,.T.);
#3784=EDGE_CURVE('',#3106,#3107,#135,.T.);
#3785=EDGE_CURVE('',#3107,#3106,#136,.T.);
#3786=EDGE_CURVE('',#3105,#3108,#2759,.T.);
#3787=EDGE_CURVE('',#3108,#3109,#137,.T.);
#3788=EDGE_CURVE('',#3110,#3109,#138,.T.);
#3789=EDGE_CURVE('',#3101,#3110,#139,.T.);
#3790=EDGE_CURVE('',#3111,#3078,#683,.T.);
#3791=EDGE_CURVE('',#3077,#3111,#684,.T.);
#3792=EDGE_CURVE('',#3079,#3112,#685,.T.);
#3793=EDGE_CURVE('',#3111,#3112,#2760,.T.);
#3794=EDGE_CURVE('',#3113,#3085,#686,.T.);
#3795=EDGE_CURVE('',#3114,#3084,#687,.T.);
#3796=EDGE_CURVE('',#3114,#3113,#2761,.T.);
#3797=EDGE_CURVE('',#3115,#3116,#688,.T.);
#3798=EDGE_CURVE('',#3116,#3117,#689,.T.);
#3799=EDGE_CURVE('',#3118,#3117,#690,.T.);
#3800=EDGE_CURVE('',#3118,#3115,#691,.T.);
#3801=EDGE_CURVE('',#3109,#3103,#2762,.T.);
#3802=EDGE_CURVE('',#3109,#3103,#140,.T.);
#3803=EDGE_CURVE('',#3119,#3120,#692,.T.);
#3804=EDGE_CURVE('',#3119,#3110,#2763,.T.);
#3805=EDGE_CURVE('',#3102,#3120,#2764,.T.);
#3806=EDGE_CURVE('',#3121,#3122,#693,.T.);
#3807=EDGE_CURVE('',#3123,#3121,#2765,.T.);
#3808=EDGE_CURVE('',#3124,#3123,#694,.T.);
#3809=EDGE_CURVE('',#3122,#3124,#2766,.T.);
#3810=EDGE_CURVE('',#3101,#3125,#695,.T.);
#3811=EDGE_CURVE('',#3126,#3125,#696,.T.);
#3812=EDGE_CURVE('',#3100,#3126,#697,.T.);
#3813=EDGE_CURVE('',#3125,#3119,#698,.T.);
#3814=EDGE_CURVE('',#3120,#3126,#699,.T.);
#3815=EDGE_CURVE('',#3109,#3127,#700,.T.);
#3816=EDGE_CURVE('',#3127,#3128,#701,.T.);
#3817=EDGE_CURVE('',#3103,#3128,#702,.T.);
#3818=EDGE_CURVE('',#3129,#3130,#703,.T.);
#3819=EDGE_CURVE('',#3129,#3131,#2767,.T.);
#3820=EDGE_CURVE('',#3131,#3132,#704,.T.);
#3821=EDGE_CURVE('',#3104,#3132,#705,.T.);
#3822=EDGE_CURVE('',#3133,#3128,#706,.T.);
#3823=EDGE_CURVE('',#3133,#3130,#2768,.T.);
#3824=EDGE_CURVE('',#3132,#3134,#707,.T.);
#3825=EDGE_CURVE('',#3108,#3134,#708,.T.);
#3826=EDGE_CURVE('',#3135,#3134,#709,.T.);
#3827=EDGE_CURVE('',#3135,#3116,#2769,.T.);
#3828=EDGE_CURVE('',#3115,#3136,#2770,.T.);
#3829=EDGE_CURVE('',#3136,#3127,#710,.T.);
#3830=EDGE_CURVE('',#3083,#3137,#711,.T.);
#3831=EDGE_CURVE('',#3137,#3133,#712,.T.);
#3832=EDGE_CURVE('',#3136,#3138,#713,.T.);
#3833=EDGE_CURVE('',#3138,#3080,#714,.T.);
#3834=EDGE_CURVE('',#3112,#3114,#715,.T.);
#3835=EDGE_CURVE('',#3082,#3139,#716,.T.);
#3836=EDGE_CURVE('',#3140,#3081,#717,.T.);
#3837=EDGE_CURVE('',#3140,#3135,#718,.T.);
#3838=EDGE_CURVE('',#3131,#3139,#719,.T.);
#3839=EDGE_CURVE('',#3141,#3142,#720,.T.);
#3840=EDGE_CURVE('',#3141,#3129,#721,.T.);
#3841=EDGE_CURVE('',#3130,#3142,#722,.T.);
#3842=EDGE_CURVE('',#3113,#3076,#723,.T.);
#3843=EDGE_CURVE('',#3138,#3118,#2771,.T.);
#3844=EDGE_CURVE('',#3117,#3140,#2772,.T.);
#3845=EDGE_CURVE('',#3139,#3141,#2773,.T.);
#3846=EDGE_CURVE('',#3142,#3137,#2774,.T.);
#3847=EDGE_CURVE('',#3143,#3144,#724,.T.);
#3848=EDGE_CURVE('',#3144,#3145,#725,.T.);
#3849=EDGE_CURVE('',#3145,#3146,#726,.T.);
#3850=EDGE_CURVE('',#3146,#3143,#727,.T.);
#3851=EDGE_CURVE('',#3121,#3147,#728,.T.);
#3852=EDGE_CURVE('',#3147,#3144,#2775,.T.);
#3853=EDGE_CURVE('',#3143,#3148,#2776,.T.);
#3854=EDGE_CURVE('',#3123,#3148,#729,.T.);
#3855=EDGE_CURVE('',#3122,#3149,#730,.T.);
#3856=EDGE_CURVE('',#3149,#3147,#731,.T.);
#3857=EDGE_CURVE('',#3145,#3149,#2777,.T.);
#3858=EDGE_CURVE('',#3124,#3150,#732,.T.);
#3859=EDGE_CURVE('',#3150,#3146,#2778,.T.);
#3860=EDGE_CURVE('',#3148,#3150,#733,.T.);
#3861=EDGE_CURVE('',#3151,#3151,#2779,.T.);
#3862=EDGE_CURVE('',#3151,#3152,#734,.T.);
#3863=EDGE_CURVE('',#3152,#3152,#2780,.T.);
#3864=EDGE_CURVE('',#3153,#3153,#2781,.T.);
#3865=EDGE_CURVE('',#3153,#3154,#735,.T.);
#3866=EDGE_CURVE('',#3154,#3154,#2782,.T.);
#3867=EDGE_CURVE('',#3155,#3155,#2783,.T.);
#3868=EDGE_CURVE('',#3155,#3156,#736,.T.);
#3869=EDGE_CURVE('',#3156,#3156,#2784,.T.);
#3870=EDGE_CURVE('',#3157,#3157,#2785,.T.);
#3871=EDGE_CURVE('',#3157,#3158,#737,.T.);
#3872=EDGE_CURVE('',#3158,#3158,#2786,.T.);
#3873=EDGE_CURVE('',#3159,#3159,#2787,.T.);
#3874=EDGE_CURVE('',#3159,#3160,#738,.T.);
#3875=EDGE_CURVE('',#3160,#3161,#141,.T.);
#3876=EDGE_CURVE('',#3161,#3160,#142,.T.);
#3877=EDGE_CURVE('',#3162,#3163,#143,.T.);
#3878=EDGE_CURVE('',#3163,#3164,#739,.T.);
#3879=EDGE_CURVE('',#3164,#3164,#2788,.T.);
#3880=EDGE_CURVE('',#3163,#3162,#144,.T.);
#3881=EDGE_CURVE('',#3165,#3166,#2789,.T.);
#3882=EDGE_CURVE('',#3167,#3166,#145,.T.);
#3883=EDGE_CURVE('',#3168,#3167,#146,.T.);
#3884=EDGE_CURVE('',#3168,#3169,#147,.T.);
#3885=EDGE_CURVE('',#3170,#3169,#148,.T.);
#3886=EDGE_CURVE('',#3170,#3171,#149,.T.);
#3887=EDGE_CURVE('',#3171,#3172,#2790,.T.);
#3888=EDGE_CURVE('',#3172,#3173,#740,.T.);
#3889=EDGE_CURVE('',#3173,#3174,#150,.T.);
#3890=EDGE_CURVE('',#3174,#3173,#151,.T.);
#3891=EDGE_CURVE('',#3172,#3175,#2791,.T.);
#3892=EDGE_CURVE('',#3175,#3176,#152,.T.);
#3893=EDGE_CURVE('',#3177,#3176,#153,.T.);
#3894=EDGE_CURVE('',#3177,#3178,#154,.T.);
#3895=EDGE_CURVE('',#3179,#3178,#155,.T.);
#3896=EDGE_CURVE('',#3165,#3179,#156,.T.);
#3897=EDGE_CURVE('',#3180,#3181,#2792,.T.);
#3898=EDGE_CURVE('',#3181,#3177,#741,.T.);
#3899=EDGE_CURVE('',#3176,#3170,#157,.T.);
#3900=EDGE_CURVE('',#3169,#3182,#742,.T.);
#3901=EDGE_CURVE('',#3182,#3183,#2793,.T.);
#3902=EDGE_CURVE('',#3180,#3183,#743,.T.);
#3903=EDGE_CURVE('',#3184,#3185,#744,.T.);
#3904=EDGE_CURVE('',#3185,#3186,#745,.T.);
#3905=EDGE_CURVE('',#3187,#3186,#746,.T.);
#3906=EDGE_CURVE('',#3187,#3184,#747,.T.);
#3907=EDGE_CURVE('',#3176,#3170,#2794,.T.);
#3908=EDGE_CURVE('',#3188,#3189,#748,.T.);
#3909=EDGE_CURVE('',#3190,#3188,#2795,.T.);
#3910=EDGE_CURVE('',#3191,#3190,#749,.T.);
#3911=EDGE_CURVE('',#3189,#3191,#2796,.T.);
#3912=EDGE_CURVE('',#3192,#3193,#2797,.T.);
#3913=EDGE_CURVE('',#3193,#3194,#750,.T.);
#3914=EDGE_CURVE('',#3195,#3194,#751,.T.);
#3915=EDGE_CURVE('',#3192,#3195,#752,.T.);
#3916=EDGE_CURVE('',#3179,#3196,#2798,.T.);
#3917=EDGE_CURVE('',#3196,#3181,#2799,.T.);
#3918=EDGE_CURVE('',#3194,#3180,#753,.T.);
#3919=EDGE_CURVE('',#3193,#3165,#158,.T.);
#3920=EDGE_CURVE('',#3182,#3197,#2800,.T.);
#3921=EDGE_CURVE('',#3197,#3167,#2801,.T.);
#3922=EDGE_CURVE('',#3166,#3192,#159,.T.);
#3923=EDGE_CURVE('',#3183,#3195,#754,.T.);
#3924=EDGE_CURVE('',#3176,#3198,#755,.T.);
#3925=EDGE_CURVE('',#3198,#3199,#756,.T.);
#3926=EDGE_CURVE('',#3170,#3199,#757,.T.);
#3927=EDGE_CURVE('',#3200,#3201,#758,.T.);
#3928=EDGE_CURVE('',#3200,#3202,#2802,.T.);
#3929=EDGE_CURVE('',#3202,#3203,#759,.T.);
#3930=EDGE_CURVE('',#3171,#3203,#760,.T.);
#3931=EDGE_CURVE('',#3204,#3199,#761,.T.);
#3932=EDGE_CURVE('',#3204,#3201,#2803,.T.);
#3933=EDGE_CURVE('',#3203,#3205,#762,.T.);
#3934=EDGE_CURVE('',#3175,#3205,#763,.T.);
#3935=EDGE_CURVE('',#3206,#3205,#764,.T.);
#3936=EDGE_CURVE('',#3206,#3185,#2804,.T.);
#3937=EDGE_CURVE('',#3184,#3207,#2805,.T.);
#3938=EDGE_CURVE('',#3207,#3198,#765,.T.);
#3939=EDGE_CURVE('',#3207,#3208,#766,.T.);
#3940=EDGE_CURVE('',#3208,#3209,#767,.T.);
#3941=EDGE_CURVE('',#3209,#3210,#768,.T.);
#3942=EDGE_CURVE('',#3210,#3211,#769,.T.);
#3943=EDGE_CURVE('',#3211,#3204,#770,.T.);
#3944=EDGE_CURVE('',#3212,#3213,#771,.T.);
#3945=EDGE_CURVE('',#3212,#3214,#772,.T.);
#3946=EDGE_CURVE('',#3215,#3214,#773,.T.);
#3947=EDGE_CURVE('',#3215,#3206,#774,.T.);
#3948=EDGE_CURVE('',#3202,#3213,#775,.T.);
#3949=EDGE_CURVE('',#3216,#3217,#776,.T.);
#3950=EDGE_CURVE('',#3216,#3200,#777,.T.);
#3951=EDGE_CURVE('',#3201,#3217,#778,.T.);
#3952=EDGE_CURVE('',#3218,#3219,#779,.T.);
#3953=EDGE_CURVE('',#3219,#3220,#780,.T.);
#3954=EDGE_CURVE('',#3221,#3220,#781,.T.);
#3955=EDGE_CURVE('',#3221,#3218,#782,.T.);
#3956=EDGE_CURVE('',#3186,#3215,#2806,.T.);
#3957=EDGE_CURVE('',#3214,#3219,#2807,.T.);
#3958=EDGE_CURVE('',#3218,#3209,#2808,.T.);
#3959=EDGE_CURVE('',#3208,#3187,#2809,.T.);
#3960=EDGE_CURVE('',#3213,#3216,#2810,.T.);
#3961=EDGE_CURVE('',#3217,#3211,#2811,.T.);
#3962=EDGE_CURVE('',#3210,#3221,#2812,.T.);
#3963=EDGE_CURVE('',#3220,#3212,#2813,.T.);
#3964=EDGE_CURVE('',#3222,#3223,#783,.T.);
#3965=EDGE_CURVE('',#3223,#3224,#784,.T.);
#3966=EDGE_CURVE('',#3224,#3225,#785,.T.);
#3967=EDGE_CURVE('',#3225,#3222,#786,.T.);
#3968=EDGE_CURVE('',#3188,#3226,#787,.T.);
#3969=EDGE_CURVE('',#3226,#3223,#2814,.T.);
#3970=EDGE_CURVE('',#3222,#3227,#2815,.T.);
#3971=EDGE_CURVE('',#3190,#3227,#788,.T.);
#3972=EDGE_CURVE('',#3189,#3228,#789,.T.);
#3973=EDGE_CURVE('',#3228,#3226,#790,.T.);
#3974=EDGE_CURVE('',#3224,#3228,#2816,.T.);
#3975=EDGE_CURVE('',#3191,#3229,#791,.T.);
#3976=EDGE_CURVE('',#3229,#3225,#2817,.T.);
#3977=EDGE_CURVE('',#3227,#3229,#792,.T.);
#3978=EDGE_CURVE('',#3197,#3168,#793,.T.);
#3979=EDGE_CURVE('',#3178,#3196,#794,.T.);
#3980=EDGE_CURVE('',#3230,#3230,#2818,.T.);
#3981=EDGE_CURVE('',#3230,#3231,#795,.T.);
#3982=EDGE_CURVE('',#3231,#3231,#2819,.T.);
#3983=EDGE_CURVE('',#3232,#3232,#2820,.T.);
#3984=EDGE_CURVE('',#3232,#3233,#796,.T.);
#3985=EDGE_CURVE('',#3233,#3233,#2821,.T.);
#3986=EDGE_CURVE('',#3234,#3234,#2822,.T.);
#3987=EDGE_CURVE('',#3234,#3235,#797,.T.);
#3988=EDGE_CURVE('',#3235,#3235,#2823,.T.);
#3989=EDGE_CURVE('',#3236,#3236,#2824,.T.);
#3990=EDGE_CURVE('',#3236,#3237,#798,.T.);
#3991=EDGE_CURVE('',#3237,#3237,#2825,.T.);
#3992=EDGE_CURVE('',#3238,#3238,#2826,.T.);
#3993=EDGE_CURVE('',#3238,#3239,#799,.T.);
#3994=EDGE_CURVE('',#3239,#3240,#160,.T.);
#3995=EDGE_CURVE('',#3240,#3239,#161,.T.);
#3996=EDGE_CURVE('',#3241,#3242,#162,.T.);
#3997=EDGE_CURVE('',#3242,#3243,#800,.T.);
#3998=EDGE_CURVE('',#3243,#3243,#2827,.T.);
#3999=EDGE_CURVE('',#3242,#3241,#163,.T.);
#4000=EDGE_CURVE('',#3244,#3245,#2828,.T.);
#4001=EDGE_CURVE('',#3246,#3245,#164,.T.);
#4002=EDGE_CURVE('',#3247,#3246,#165,.T.);
#4003=EDGE_CURVE('',#3247,#3248,#166,.T.);
#4004=EDGE_CURVE('',#3249,#3248,#167,.T.);
#4005=EDGE_CURVE('',#3249,#3250,#168,.T.);
#4006=EDGE_CURVE('',#3251,#3250,#169,.T.);
#4007=EDGE_CURVE('',#3251,#3252,#170,.T.);
#4008=EDGE_CURVE('',#3252,#3253,#2829,.T.);
#4009=EDGE_CURVE('',#3253,#3254,#801,.T.);
#4010=EDGE_CURVE('',#3254,#3255,#171,.T.);
#4011=EDGE_CURVE('',#3255,#3254,#172,.T.);
#4012=EDGE_CURVE('',#3253,#3256,#2830,.T.);
#4013=EDGE_CURVE('',#3256,#3257,#173,.T.);
#4014=EDGE_CURVE('',#3258,#3257,#174,.T.);
#4015=EDGE_CURVE('',#3258,#3259,#175,.T.);
#4016=EDGE_CURVE('',#3260,#3259,#176,.T.);
#4017=EDGE_CURVE('',#3260,#3261,#177,.T.);
#4018=EDGE_CURVE('',#3262,#3261,#178,.T.);
#4019=EDGE_CURVE('',#3244,#3262,#179,.T.);
#4020=EDGE_CURVE('',#3248,#3263,#802,.T.);
#4021=EDGE_CURVE('',#3264,#3263,#2831,.T.);
#4022=EDGE_CURVE('',#3264,#3249,#803,.T.);
#4023=EDGE_CURVE('',#3265,#3266,#2832,.T.);
#4024=EDGE_CURVE('',#3265,#3260,#804,.T.);
#4025=EDGE_CURVE('',#3259,#3266,#805,.T.);
#4026=EDGE_CURVE('',#3267,#3268,#2833,.T.);
#4027=EDGE_CURVE('',#3245,#3267,#180,.T.);
#4028=EDGE_CURVE('',#3268,#3244,#181,.T.);
#4029=EDGE_CURVE('',#3269,#3269,#182,.T.);
#4030=EDGE_CURVE('',#3270,#3271,#2834,.T.);
#4031=EDGE_CURVE('',#3271,#3258,#806,.T.);
#4032=EDGE_CURVE('',#3257,#3251,#183,.T.);
#4033=EDGE_CURVE('',#3250,#3272,#807,.T.);
#4034=EDGE_CURVE('',#3272,#3273,#2835,.T.);
#4035=EDGE_CURVE('',#3270,#3273,#808,.T.);
#4036=EDGE_CURVE('',#3274,#3275,#809,.T.);
#4037=EDGE_CURVE('',#3275,#3276,#810,.T.);
#4038=EDGE_CURVE('',#3277,#3276,#811,.T.);
#4039=EDGE_CURVE('',#3277,#3274,#812,.T.);
#4040=EDGE_CURVE('',#3257,#3251,#2836,.T.);
#4041=EDGE_CURVE('',#3278,#3279,#813,.T.);
#4042=EDGE_CURVE('',#3280,#3278,#2837,.T.);
#4043=EDGE_CURVE('',#3281,#3280,#814,.T.);
#4044=EDGE_CURVE('',#3279,#3281,#2838,.T.);
#4045=EDGE_CURVE('',#3268,#3282,#815,.T.);
#4046=EDGE_CURVE('',#3283,#3282,#816,.T.);
#4047=EDGE_CURVE('',#3267,#3283,#817,.T.);
#4048=EDGE_CURVE('',#3262,#3284,#2839,.T.);
#4049=EDGE_CURVE('',#3284,#3265,#2840,.T.);
#4050=EDGE_CURVE('',#3266,#3271,#2841,.T.);
#4051=EDGE_CURVE('',#3282,#3270,#818,.T.);
#4052=EDGE_CURVE('',#3263,#3285,#2842,.T.);
#4053=EDGE_CURVE('',#3285,#3246,#2843,.T.);
#4054=EDGE_CURVE('',#3273,#3283,#819,.T.);
#4055=EDGE_CURVE('',#3272,#3264,#2844,.T.);
#4056=EDGE_CURVE('',#3257,#3286,#820,.T.);
#4057=EDGE_CURVE('',#3286,#3287,#821,.T.);
#4058=EDGE_CURVE('',#3251,#3287,#822,.T.);
#4059=EDGE_CURVE('',#3288,#3289,#823,.T.);
#4060=EDGE_CURVE('',#3288,#3290,#2845,.T.);
#4061=EDGE_CURVE('',#3290,#3291,#824,.T.);
#4062=EDGE_CURVE('',#3252,#3291,#825,.T.);
#4063=EDGE_CURVE('',#3292,#3287,#826,.T.);
#4064=EDGE_CURVE('',#3292,#3289,#2846,.T.);
#4065=EDGE_CURVE('',#3291,#3293,#827,.T.);
#4066=EDGE_CURVE('',#3256,#3293,#828,.T.);
#4067=EDGE_CURVE('',#3294,#3293,#829,.T.);
#4068=EDGE_CURVE('',#3294,#3275,#2847,.T.);
#4069=EDGE_CURVE('',#3274,#3295,#2848,.T.);
#4070=EDGE_CURVE('',#3295,#3286,#830,.T.);
#4071=EDGE_CURVE('',#3295,#3296,#831,.T.);
#4072=EDGE_CURVE('',#3296,#3297,#832,.T.);
#4073=EDGE_CURVE('',#3297,#3298,#833,.T.);
#4074=EDGE_CURVE('',#3298,#3299,#834,.T.);
#4075=EDGE_CURVE('',#3299,#3292,#835,.T.);
#4076=EDGE_CURVE('',#3300,#3301,#836,.T.);
#4077=EDGE_CURVE('',#3300,#3302,#837,.T.);
#4078=EDGE_CURVE('',#3303,#3302,#838,.T.);
#4079=EDGE_CURVE('',#3303,#3294,#839,.T.);
#4080=EDGE_CURVE('',#3290,#3301,#840,.T.);
#4081=EDGE_CURVE('',#3304,#3305,#841,.T.);
#4082=EDGE_CURVE('',#3304,#3288,#842,.T.);
#4083=EDGE_CURVE('',#3289,#3305,#843,.T.);
#4084=EDGE_CURVE('',#3306,#3307,#844,.T.);
#4085=EDGE_CURVE('',#3307,#3308,#845,.T.);
#4086=EDGE_CURVE('',#3309,#3308,#846,.T.);
#4087=EDGE_CURVE('',#3309,#3306,#847,.T.);
#4088=EDGE_CURVE('',#3276,#3303,#2849,.T.);
#4089=EDGE_CURVE('',#3302,#3307,#2850,.T.);
#4090=EDGE_CURVE('',#3306,#3297,#2851,.T.);
#4091=EDGE_CURVE('',#3296,#3277,#2852,.T.);
#4092=EDGE_CURVE('',#3301,#3304,#2853,.T.);
#4093=EDGE_CURVE('',#3305,#3299,#2854,.T.);
#4094=EDGE_CURVE('',#3298,#3309,#2855,.T.);
#4095=EDGE_CURVE('',#3308,#3300,#2856,.T.);
#4096=EDGE_CURVE('',#3310,#3311,#848,.T.);
#4097=EDGE_CURVE('',#3311,#3312,#849,.T.);
#4098=EDGE_CURVE('',#3312,#3313,#850,.T.);
#4099=EDGE_CURVE('',#3313,#3310,#851,.T.);
#4100=EDGE_CURVE('',#3278,#3314,#852,.T.);
#4101=EDGE_CURVE('',#3314,#3311,#2857,.T.);
#4102=EDGE_CURVE('',#3310,#3315,#2858,.T.);
#4103=EDGE_CURVE('',#3280,#3315,#853,.T.);
#4104=EDGE_CURVE('',#3279,#3316,#854,.T.);
#4105=EDGE_CURVE('',#3316,#3314,#855,.T.);
#4106=EDGE_CURVE('',#3312,#3316,#2859,.T.);
#4107=EDGE_CURVE('',#3281,#3317,#856,.T.);
#4108=EDGE_CURVE('',#3317,#3313,#2860,.T.);
#4109=EDGE_CURVE('',#3315,#3317,#857,.T.);
#4110=EDGE_CURVE('',#3261,#3284,#858,.T.);
#4111=EDGE_CURVE('',#3285,#3247,#859,.T.);
#4112=EDGE_CURVE('',#3318,#3318,#2861,.T.);
#4113=EDGE_CURVE('',#3318,#3319,#860,.T.);
#4114=EDGE_CURVE('',#3319,#3319,#2862,.T.);
#4115=EDGE_CURVE('',#3320,#3320,#2863,.T.);
#4116=EDGE_CURVE('',#3320,#3321,#861,.T.);
#4117=EDGE_CURVE('',#3321,#3321,#2864,.T.);
#4118=EDGE_CURVE('',#3322,#3322,#2865,.T.);
#4119=EDGE_CURVE('',#3322,#3323,#862,.T.);
#4120=EDGE_CURVE('',#3323,#3323,#2866,.T.);
#4121=EDGE_CURVE('',#3324,#3325,#863,.T.);
#4122=EDGE_CURVE('',#3326,#3324,#864,.T.);
#4123=EDGE_CURVE('',#3327,#3326,#865,.T.);
#4124=EDGE_CURVE('',#3325,#3327,#866,.T.);
#4125=EDGE_CURVE('',#3328,#3329,#2867,.T.);
#4126=EDGE_CURVE('',#3329,#3324,#867,.T.);
#4127=EDGE_CURVE('',#3328,#3325,#868,.T.);
#4128=EDGE_CURVE('',#3330,#3327,#869,.T.);
#4129=EDGE_CURVE('',#3330,#3328,#870,.T.);
#4130=EDGE_CURVE('',#3331,#3326,#871,.T.);
#4131=EDGE_CURVE('',#3331,#3330,#2868,.T.);
#4132=EDGE_CURVE('',#3329,#3331,#872,.T.);
#4133=EDGE_CURVE('',#3332,#3332,#2869,.T.);
#4134=EDGE_CURVE('',#3332,#3333,#873,.T.);
#4135=EDGE_CURVE('',#3333,#3333,#2870,.T.);
#4136=EDGE_CURVE('',#3334,#3335,#2871,.T.);
#4137=EDGE_CURVE('',#3336,#3334,#874,.T.);
#4138=EDGE_CURVE('',#3337,#3336,#2872,.T.);
#4139=EDGE_CURVE('',#3335,#3337,#875,.T.);
#4140=EDGE_CURVE('',#3338,#3338,#2873,.T.);
#4141=EDGE_CURVE('',#3338,#3339,#876,.T.);
#4142=EDGE_CURVE('',#3339,#3339,#2874,.T.);
#4143=EDGE_CURVE('',#3340,#3341,#877,.T.);
#4144=EDGE_CURVE('',#3342,#3340,#878,.T.);
#4145=EDGE_CURVE('',#3343,#3342,#879,.T.);
#4146=EDGE_CURVE('',#3341,#3343,#880,.T.);
#4147=EDGE_CURVE('',#3337,#3340,#881,.T.);
#4148=EDGE_CURVE('',#3336,#3342,#882,.T.);
#4149=EDGE_CURVE('',#3335,#3341,#883,.T.);
#4150=EDGE_CURVE('',#3334,#3343,#884,.T.);
#4151=EDGE_CURVE('',#3344,#3344,#2875,.T.);
#4152=EDGE_CURVE('',#3344,#3345,#885,.T.);
#4153=EDGE_CURVE('',#3345,#3345,#2876,.T.);
#4154=EDGE_CURVE('',#3346,#3346,#2877,.T.);
#4155=EDGE_CURVE('',#3346,#3347,#886,.T.);
#4156=EDGE_CURVE('',#3347,#3347,#2878,.T.);
#4157=EDGE_CURVE('',#3348,#3348,#2879,.T.);
#4158=EDGE_CURVE('',#3348,#3349,#887,.T.);
#4159=EDGE_CURVE('',#3349,#3349,#2880,.T.);
#4160=EDGE_CURVE('',#3350,#3351,#888,.T.);
#4161=EDGE_CURVE('',#3352,#3350,#889,.T.);
#4162=EDGE_CURVE('',#3353,#3352,#890,.T.);
#4163=EDGE_CURVE('',#3351,#3353,#891,.T.);
#4164=EDGE_CURVE('',#3354,#3355,#2881,.T.);
#4165=EDGE_CURVE('',#3355,#3350,#892,.T.);
#4166=EDGE_CURVE('',#3354,#3351,#893,.T.);
#4167=EDGE_CURVE('',#3356,#3353,#894,.T.);
#4168=EDGE_CURVE('',#3356,#3354,#895,.T.);
#4169=EDGE_CURVE('',#3357,#3352,#896,.T.);
#4170=EDGE_CURVE('',#3357,#3356,#2882,.T.);
#4171=EDGE_CURVE('',#3355,#3357,#897,.T.);
#4172=EDGE_CURVE('',#3358,#3358,#2883,.T.);
#4173=EDGE_CURVE('',#3358,#3359,#898,.T.);
#4174=EDGE_CURVE('',#3359,#3359,#2884,.T.);
#4175=EDGE_CURVE('',#3360,#3361,#2885,.T.);
#4176=EDGE_CURVE('',#3362,#3360,#899,.T.);
#4177=EDGE_CURVE('',#3363,#3362,#2886,.T.);
#4178=EDGE_CURVE('',#3361,#3363,#900,.T.);
#4179=EDGE_CURVE('',#3364,#3364,#2887,.T.);
#4180=EDGE_CURVE('',#3364,#3365,#901,.T.);
#4181=EDGE_CURVE('',#3365,#3365,#2888,.T.);
#4182=EDGE_CURVE('',#3366,#3367,#902,.T.);
#4183=EDGE_CURVE('',#3368,#3366,#903,.T.);
#4184=EDGE_CURVE('',#3369,#3368,#904,.T.);
#4185=EDGE_CURVE('',#3367,#3369,#905,.T.);
#4186=EDGE_CURVE('',#3363,#3366,#906,.T.);
#4187=EDGE_CURVE('',#3362,#3368,#907,.T.);
#4188=EDGE_CURVE('',#3361,#3367,#908,.T.);
#4189=EDGE_CURVE('',#3360,#3369,#909,.T.);
#4190=EDGE_CURVE('',#3370,#3370,#2889,.T.);
#4191=EDGE_CURVE('',#3370,#3371,#910,.T.);
#4192=EDGE_CURVE('',#3371,#3371,#2890,.T.);
#4193=EDGE_CURVE('',#3372,#3372,#2891,.T.);
#4194=EDGE_CURVE('',#3372,#3373,#911,.T.);
#4195=EDGE_CURVE('',#3373,#3373,#2892,.T.);
#4196=EDGE_CURVE('',#3374,#3374,#2893,.T.);
#4197=EDGE_CURVE('',#3374,#3375,#912,.T.);
#4198=EDGE_CURVE('',#3375,#3375,#2894,.T.);
#4199=EDGE_CURVE('',#3376,#3377,#913,.T.);
#4200=EDGE_CURVE('',#3378,#3376,#914,.T.);
#4201=EDGE_CURVE('',#3379,#3378,#915,.T.);
#4202=EDGE_CURVE('',#3377,#3379,#916,.T.);
#4203=EDGE_CURVE('',#3380,#3381,#2895,.T.);
#4204=EDGE_CURVE('',#3381,#3376,#917,.T.);
#4205=EDGE_CURVE('',#3380,#3377,#918,.T.);
#4206=EDGE_CURVE('',#3382,#3379,#919,.T.);
#4207=EDGE_CURVE('',#3382,#3380,#920,.T.);
#4208=EDGE_CURVE('',#3383,#3378,#921,.T.);
#4209=EDGE_CURVE('',#3383,#3382,#2896,.T.);
#4210=EDGE_CURVE('',#3381,#3383,#922,.T.);
#4211=EDGE_CURVE('',#3384,#3384,#2897,.T.);
#4212=EDGE_CURVE('',#3384,#3385,#923,.T.);
#4213=EDGE_CURVE('',#3385,#3385,#2898,.T.);
#4214=EDGE_CURVE('',#3386,#3387,#2899,.T.);
#4215=EDGE_CURVE('',#3388,#3386,#924,.T.);
#4216=EDGE_CURVE('',#3389,#3388,#2900,.T.);
#4217=EDGE_CURVE('',#3387,#3389,#925,.T.);
#4218=EDGE_CURVE('',#3390,#3390,#2901,.T.);
#4219=EDGE_CURVE('',#3390,#3391,#926,.T.);
#4220=EDGE_CURVE('',#3391,#3391,#2902,.T.);
#4221=EDGE_CURVE('',#3392,#3393,#927,.T.);
#4222=EDGE_CURVE('',#3394,#3392,#928,.T.);
#4223=EDGE_CURVE('',#3395,#3394,#929,.T.);
#4224=EDGE_CURVE('',#3393,#3395,#930,.T.);
#4225=EDGE_CURVE('',#3389,#3392,#931,.T.);
#4226=EDGE_CURVE('',#3388,#3394,#932,.T.);
#4227=EDGE_CURVE('',#3387,#3393,#933,.T.);
#4228=EDGE_CURVE('',#3386,#3395,#934,.T.);
#4229=EDGE_CURVE('',#3396,#3396,#2903,.T.);
#4230=EDGE_CURVE('',#3396,#3397,#935,.T.);
#4231=EDGE_CURVE('',#3397,#3397,#2904,.T.);
#4232=EDGE_CURVE('',#3398,#3398,#2905,.T.);
#4233=EDGE_CURVE('',#3398,#3399,#936,.T.);
#4234=EDGE_CURVE('',#3399,#3399,#2906,.T.);
#4235=EDGE_CURVE('',#3400,#3400,#2907,.T.);
#4236=EDGE_CURVE('',#3400,#3401,#937,.T.);
#4237=EDGE_CURVE('',#3401,#3401,#2908,.T.);
#4238=EDGE_CURVE('',#3402,#3403,#938,.T.);
#4239=EDGE_CURVE('',#3402,#3404,#939,.T.);
#4240=EDGE_CURVE('',#3404,#3405,#940,.T.);
#4241=EDGE_CURVE('',#3405,#3403,#941,.T.);
#4242=EDGE_CURVE('',#3406,#3407,#942,.T.);
#4243=EDGE_CURVE('',#3408,#3407,#943,.T.);
#4244=EDGE_CURVE('',#3405,#3408,#944,.T.);
#4245=EDGE_CURVE('',#3404,#3409,#945,.T.);
#4246=EDGE_CURVE('',#3409,#3406,#946,.T.);
#4247=EDGE_CURVE('',#3407,#3410,#947,.T.);
#4248=EDGE_CURVE('',#3411,#3410,#948,.T.);
#4249=EDGE_CURVE('',#3408,#3411,#949,.T.);
#4250=EDGE_CURVE('',#3410,#3412,#950,.T.);
#4251=EDGE_CURVE('',#3413,#3412,#951,.T.);
#4252=EDGE_CURVE('',#3414,#3413,#952,.T.);
#4253=EDGE_CURVE('',#3415,#3414,#953,.T.);
#4254=EDGE_CURVE('',#3415,#3411,#954,.T.);
#4255=EDGE_CURVE('',#3412,#3406,#955,.T.);
#4256=EDGE_CURVE('',#3413,#3409,#956,.T.);
#4257=EDGE_CURVE('',#3416,#3402,#957,.T.);
#4258=EDGE_CURVE('',#3417,#3416,#958,.T.);
#4259=EDGE_CURVE('',#3418,#3417,#959,.T.);
#4260=EDGE_CURVE('',#3414,#3418,#960,.T.);
#4261=EDGE_CURVE('',#3419,#3420,#961,.T.);
#4262=EDGE_CURVE('',#3403,#3419,#962,.T.);
#4263=EDGE_CURVE('',#3421,#3415,#963,.T.);
#4264=EDGE_CURVE('',#3420,#3421,#964,.T.);
#4265=EDGE_CURVE('',#3421,#3418,#965,.T.);
#4266=EDGE_CURVE('',#3416,#3419,#966,.T.);
#4267=EDGE_CURVE('',#3417,#3420,#967,.T.);
#4268=EDGE_CURVE('',#3422,#3422,#2909,.T.);
#4269=EDGE_CURVE('',#3422,#3423,#968,.T.);
#4270=EDGE_CURVE('',#3423,#3424,#184,.T.);
#4271=EDGE_CURVE('',#3424,#3423,#185,.T.);
#4272=EDGE_CURVE('',#3425,#3426,#186,.T.);
#4273=EDGE_CURVE('',#3426,#3427,#969,.T.);
#4274=EDGE_CURVE('',#3427,#3427,#2910,.T.);
#4275=EDGE_CURVE('',#3426,#3425,#187,.T.);
#4276=EDGE_CURVE('',#3428,#3428,#2911,.T.);
#4277=EDGE_CURVE('',#3428,#3429,#2912,.T.);
#4278=EDGE_CURVE('',#3430,#3430,#188,.T.);
#4279=EDGE_CURVE('',#3430,#3428,#11,.T.);
#4280=EDGE_CURVE('',#3431,#3432,#2913,.T.);
#4281=EDGE_CURVE('',#3432,#3433,#970,.T.);
#4282=EDGE_CURVE('',#3433,#3434,#2914,.T.);
#4283=EDGE_CURVE('',#3434,#3431,#971,.T.);
#4284=EDGE_CURVE('',#3435,#3436,#972,.T.);
#4285=EDGE_CURVE('',#3436,#3437,#973,.T.);
#4286=EDGE_CURVE('',#3437,#3438,#974,.T.);
#4287=EDGE_CURVE('',#3438,#3435,#975,.T.);
#4288=EDGE_CURVE('',#3437,#3434,#976,.T.);
#4289=EDGE_CURVE('',#3436,#3431,#977,.T.);
#4290=EDGE_CURVE('',#3438,#3433,#978,.T.);
#4291=EDGE_CURVE('',#3435,#3432,#979,.T.);
#4292=EDGE_CURVE('',#3439,#3439,#2915,.T.);
#4293=EDGE_CURVE('',#3439,#3440,#980,.T.);
#4294=EDGE_CURVE('',#3440,#3440,#2916,.T.);
#4295=EDGE_CURVE('',#3441,#3441,#2917,.T.);
#4296=EDGE_CURVE('',#3441,#3442,#981,.T.);
#4297=EDGE_CURVE('',#3442,#3442,#2918,.T.);
#4298=EDGE_CURVE('',#3443,#3443,#2919,.T.);
#4299=EDGE_CURVE('',#3443,#3444,#982,.T.);
#4300=EDGE_CURVE('',#3444,#3444,#2920,.T.);
#4301=EDGE_CURVE('',#3445,#3445,#2921,.T.);
#4302=EDGE_CURVE('',#3445,#3446,#983,.T.);
#4303=EDGE_CURVE('',#3446,#3446,#2922,.T.);
#4304=EDGE_CURVE('',#3444,#3447,#2923,.T.);
#4305=EDGE_CURVE('',#3448,#3447,#2924,.T.);
#4306=EDGE_CURVE('',#3449,#3448,#2925,.T.);
#4307=EDGE_CURVE('',#3450,#3449,#2926,.T.);
#4308=EDGE_CURVE('',#3450,#3445,#2927,.T.);
#4309=EDGE_CURVE('',#3451,#3450,#2928,.T.);
#4310=EDGE_CURVE('',#3452,#3451,#2929,.T.);
#4311=EDGE_CURVE('',#3447,#3452,#2930,.T.);
#4312=EDGE_CURVE('',#3453,#3454,#2931,.T.);
#4313=EDGE_CURVE('',#3455,#3453,#2932,.T.);
#4314=EDGE_CURVE('',#3456,#3455,#2933,.T.);
#4315=EDGE_CURVE('',#3454,#3456,#2934,.T.);
#4316=EDGE_CURVE('',#3457,#3458,#2935,.T.);
#4317=EDGE_CURVE('',#3458,#3459,#2936,.T.);
#4318=EDGE_CURVE('',#3460,#3459,#2937,.T.);
#4319=EDGE_CURVE('',#3457,#3460,#2938,.T.);
#4320=EDGE_CURVE('',#3461,#3462,#984,.T.);
#4321=EDGE_CURVE('',#3461,#3463,#985,.T.);
#4322=EDGE_CURVE('',#3463,#3464,#986,.T.);
#4323=EDGE_CURVE('',#3464,#3462,#987,.T.);
#4324=EDGE_CURVE('',#3465,#3457,#988,.T.);
#4325=EDGE_CURVE('',#3465,#3466,#989,.T.);
#4326=EDGE_CURVE('',#3466,#3458,#990,.T.);
#4327=EDGE_CURVE('',#3467,#3460,#991,.T.);
#4328=EDGE_CURVE('',#3465,#3467,#992,.T.);
#4329=EDGE_CURVE('',#3468,#3459,#993,.T.);
#4330=EDGE_CURVE('',#3467,#3468,#994,.T.);
#4331=EDGE_CURVE('',#3466,#3468,#995,.T.);
#4332=EDGE_CURVE('',#3452,#3469,#996,.T.);
#4333=EDGE_CURVE('',#3448,#3469,#997,.T.);
#4334=EDGE_CURVE('',#3451,#3470,#998,.T.);
#4335=EDGE_CURVE('',#3469,#3470,#999,.T.);
#4336=EDGE_CURVE('',#3470,#3449,#1000,.T.);
#4337=EDGE_CURVE('',#3471,#3472,#1001,.T.);
#4338=EDGE_CURVE('',#3472,#3462,#1002,.T.);
#4339=EDGE_CURVE('',#3464,#3456,#1003,.T.);
#4340=EDGE_CURVE('',#3473,#3455,#1004,.T.);
#4341=EDGE_CURVE('',#3474,#3473,#1005,.T.);
#4342=EDGE_CURVE('',#3474,#3471,#1006,.T.);
#4343=EDGE_CURVE('',#3475,#3453,#1007,.T.);
#4344=EDGE_CURVE('',#3473,#3475,#1008,.T.);
#4345=EDGE_CURVE('',#3476,#3461,#1009,.T.);
#4346=EDGE_CURVE('',#3477,#3476,#1010,.T.);
#4347=EDGE_CURVE('',#3478,#3477,#1011,.T.);
#4348=EDGE_CURVE('',#3475,#3478,#1012,.T.);
#4349=EDGE_CURVE('',#3463,#3454,#1013,.T.);
#4350=EDGE_CURVE('',#3474,#3478,#1014,.T.);
#4351=EDGE_CURVE('',#3471,#3477,#1015,.T.);
#4352=EDGE_CURVE('',#3472,#3476,#1016,.T.);
#4353=EDGE_CURVE('',#3479,#3479,#2939,.T.);
#4354=EDGE_CURVE('',#3479,#3480,#1017,.T.);
#4355=EDGE_CURVE('',#3480,#3480,#2940,.T.);
#4356=EDGE_CURVE('',#3481,#3481,#2941,.T.);
#4357=EDGE_CURVE('',#3481,#3482,#1018,.T.);
#4358=EDGE_CURVE('',#3482,#3483,#189,.T.);
#4359=EDGE_CURVE('',#3483,#3482,#190,.T.);
#4360=EDGE_CURVE('',#3484,#3485,#191,.T.);
#4361=EDGE_CURVE('',#3485,#3486,#1019,.T.);
#4362=EDGE_CURVE('',#3486,#3486,#2942,.T.);
#4363=EDGE_CURVE('',#3485,#3484,#192,.T.);
#4364=EDGE_CURVE('',#3487,#3488,#1020,.T.);
#4365=EDGE_CURVE('',#3488,#3489,#1021,.T.);
#4366=EDGE_CURVE('',#3489,#3490,#1022,.T.);
#4367=EDGE_CURVE('',#3490,#3487,#2943,.T.);
#4368=EDGE_CURVE('',#3491,#3492,#1023,.T.);
#4369=EDGE_CURVE('',#3491,#3488,#2944,.T.);
#4370=EDGE_CURVE('',#3487,#3493,#193,.T.);
#4371=EDGE_CURVE('',#3494,#3493,#1024,.T.);
#4372=EDGE_CURVE('',#3494,#3495,#194,.T.);
#4373=EDGE_CURVE('',#3496,#3495,#1025,.T.);
#4374=EDGE_CURVE('',#3492,#3496,#2945,.T.);
#4375=EDGE_CURVE('',#3489,#3497,#2946,.T.);
#4376=EDGE_CURVE('',#3498,#3497,#1026,.T.);
#4377=EDGE_CURVE('',#3499,#3498,#2947,.T.);
#4378=EDGE_CURVE('',#3500,#3499,#1027,.T.);
#4379=EDGE_CURVE('',#3500,#3490,#195,.T.);
#4380=EDGE_CURVE('',#3495,#3500,#2948,.T.);
#4381=EDGE_CURVE('',#3501,#3494,#12,.T.);
#4382=EDGE_CURVE('',#3502,#3501,#2949,.T.);
#4383=EDGE_CURVE('',#3503,#3502,#196,.T.);
#4384=EDGE_CURVE('',#3504,#3503,#197,.T.);
#4385=EDGE_CURVE('',#3505,#3504,#198,.T.);
#4386=EDGE_CURVE('',#3506,#3505,#2950,.T.);
#4387=EDGE_CURVE('',#3493,#3506,#13,.T.);
#4388=EDGE_CURVE('',#3506,#3501,#1028,.T.);
#4389=EDGE_CURVE('',#3496,#3499,#1029,.T.);
#4390=EDGE_CURVE('',#3507,#3508,#1030,.T.);
#4391=EDGE_CURVE('',#3507,#3504,#2951,.T.);
#4392=EDGE_CURVE('',#3503,#3508,#2952,.T.);
#4393=EDGE_CURVE('',#3509,#3507,#1031,.T.);
#4394=EDGE_CURVE('',#3505,#3509,#1032,.T.);
#4395=EDGE_CURVE('',#3502,#3510,#1033,.T.);
#4396=EDGE_CURVE('',#3508,#3510,#1034,.T.);
#4397=EDGE_CURVE('',#3510,#3509,#1035,.T.);
#4398=EDGE_CURVE('',#3511,#3491,#1036,.T.);
#4399=EDGE_CURVE('',#3512,#3492,#1037,.T.);
#4400=EDGE_CURVE('',#3511,#3512,#1038,.T.);
#4401=EDGE_CURVE('',#3513,#3512,#1039,.T.);
#4402=EDGE_CURVE('',#3514,#3513,#1040,.T.);
#4403=EDGE_CURVE('',#3514,#3511,#1041,.T.);
#4404=EDGE_CURVE('',#3498,#3513,#1042,.T.);
#4405=EDGE_CURVE('',#3497,#3514,#1043,.T.);
#4406=EDGE_CURVE('',#3515,#3515,#2953,.T.);
#4407=EDGE_CURVE('',#3515,#3516,#1044,.T.);
#4408=EDGE_CURVE('',#3516,#3517,#199,.T.);
#4409=EDGE_CURVE('',#3517,#3516,#200,.T.);
#4410=EDGE_CURVE('',#3518,#3519,#201,.T.);
#4411=EDGE_CURVE('',#3519,#3520,#1045,.T.);
#4412=EDGE_CURVE('',#3520,#3520,#2954,.T.);
#4413=EDGE_CURVE('',#3519,#3518,#202,.T.);
#4414=EDGE_CURVE('',#3521,#3522,#203,.T.);
#4415=EDGE_CURVE('',#3523,#3522,#392,.T.);
#4416=EDGE_CURVE('',#3524,#3523,#1046,.T.);
#4417=EDGE_CURVE('',#3525,#3524,#393,.T.);
#4418=EDGE_CURVE('',#3525,#3526,#1047,.T.);
#4419=EDGE_CURVE('',#3527,#3526,#394,.T.);
#4420=EDGE_CURVE('',#3528,#3527,#1048,.T.);
#4421=EDGE_CURVE('',#3529,#3528,#395,.T.);
#4422=EDGE_CURVE('',#3530,#3529,#1049,.T.);
#4423=EDGE_CURVE('',#3521,#3530,#396,.T.);
#4424=EDGE_CURVE('',#3531,#3531,#2955,.T.);
#4425=EDGE_CURVE('',#3531,#3532,#1050,.T.);
#4426=EDGE_CURVE('',#3532,#3532,#2956,.T.);
#4427=EDGE_CURVE('',#3533,#3533,#2957,.T.);
#4428=EDGE_CURVE('',#3533,#3534,#1051,.T.);
#4429=EDGE_CURVE('',#3534,#3534,#2958,.T.);
#4430=EDGE_CURVE('',#3535,#3535,#2959,.T.);
#4431=EDGE_CURVE('',#3535,#3536,#1052,.T.);
#4432=EDGE_CURVE('',#3536,#3536,#2960,.T.);
#4433=EDGE_CURVE('',#3537,#3538,#204,.T.);
#4434=EDGE_CURVE('',#3537,#3539,#205,.T.);
#4435=EDGE_CURVE('',#3539,#3540,#206,.T.);
#4436=EDGE_CURVE('',#3541,#3540,#14,.T.);
#4437=EDGE_CURVE('',#3542,#3541,#2961,.T.);
#4438=EDGE_CURVE('',#3543,#3542,#15,.T.);
#4439=EDGE_CURVE('',#3543,#3544,#207,.T.);
#4440=EDGE_CURVE('',#3544,#3545,#208,.T.);
#4441=EDGE_CURVE('',#3546,#3545,#209,.T.);
#4442=EDGE_CURVE('',#3546,#3547,#16,.T.);
#4443=EDGE_CURVE('',#3547,#3548,#2962,.T.);
#4444=EDGE_CURVE('',#3548,#3538,#210,.T.);
#4445=EDGE_CURVE('',#3549,#3523,#1053,.T.);
#4446=EDGE_CURVE('',#3522,#3549,#1054,.T.);
#4447=EDGE_CURVE('',#3524,#3550,#1055,.T.);
#4448=EDGE_CURVE('',#3549,#3550,#2963,.T.);
#4449=EDGE_CURVE('',#3551,#3530,#1056,.T.);
#4450=EDGE_CURVE('',#3552,#3529,#1057,.T.);
#4451=EDGE_CURVE('',#3552,#3551,#2964,.T.);
#4452=EDGE_CURVE('',#3553,#3554,#1058,.T.);
#4453=EDGE_CURVE('',#3554,#3555,#1059,.T.);
#4454=EDGE_CURVE('',#3556,#3555,#1060,.T.);
#4455=EDGE_CURVE('',#3556,#3553,#1061,.T.);
#4456=EDGE_CURVE('',#3557,#3546,#2965,.T.);
#4457=EDGE_CURVE('',#3557,#3546,#211,.T.);
#4458=EDGE_CURVE('',#3558,#3559,#2966,.T.);
#4459=EDGE_CURVE('',#3559,#3537,#1062,.T.);
#4460=EDGE_CURVE('',#3538,#3557,#2967,.T.);
#4461=EDGE_CURVE('',#3545,#3560,#1063,.T.);
#4462=EDGE_CURVE('',#3560,#3561,#2968,.T.);
#4463=EDGE_CURVE('',#3558,#3561,#1064,.T.);
#4464=EDGE_CURVE('',#3543,#3540,#1065,.T.);
#4465=EDGE_CURVE('',#3541,#3542,#1066,.T.);
#4466=EDGE_CURVE('',#3562,#3563,#2969,.T.);
#4467=EDGE_CURVE('',#3562,#3559,#2970,.T.);
#4468=EDGE_CURVE('',#3564,#3558,#1067,.T.);
#4469=EDGE_CURVE('',#3565,#3564,#1068,.T.);
#4470=EDGE_CURVE('',#3565,#3563,#1069,.T.);
#4471=EDGE_CURVE('',#3560,#3566,#2971,.T.);
#4472=EDGE_CURVE('',#3567,#3566,#2972,.T.);
#4473=EDGE_CURVE('',#3568,#3567,#1070,.T.);
#4474=EDGE_CURVE('',#3569,#3568,#1071,.T.);
#4475=EDGE_CURVE('',#3561,#3569,#1072,.T.);
#4476=EDGE_CURVE('',#3564,#3569,#1073,.T.);
#4477=EDGE_CURVE('',#3570,#3557,#2973,.T.);
#4478=EDGE_CURVE('',#3570,#3571,#1074,.T.);
#4479=EDGE_CURVE('',#3571,#3572,#1075,.T.);
#4480=EDGE_CURVE('',#3546,#3572,#1076,.T.);
#4481=EDGE_CURVE('',#3573,#3574,#1077,.T.);
#4482=EDGE_CURVE('',#3573,#3575,#2974,.T.);
#4483=EDGE_CURVE('',#3575,#3576,#1078,.T.);
#4484=EDGE_CURVE('',#3547,#3576,#1079,.T.);
#4485=EDGE_CURVE('',#3577,#3572,#1080,.T.);
#4486=EDGE_CURVE('',#3577,#3574,#2975,.T.);
#4487=EDGE_CURVE('',#3576,#3578,#1081,.T.);
#4488=EDGE_CURVE('',#3548,#3578,#1082,.T.);
#4489=EDGE_CURVE('',#3579,#3578,#1083,.T.);
#4490=EDGE_CURVE('',#3579,#3554,#2976,.T.);
#4491=EDGE_CURVE('',#3553,#3580,#2977,.T.);
#4492=EDGE_CURVE('',#3580,#3571,#1084,.T.);
#4493=EDGE_CURVE('',#3538,#3570,#1085,.T.);
#4494=EDGE_CURVE('',#3528,#3581,#1086,.T.);
#4495=EDGE_CURVE('',#3581,#3577,#1087,.T.);
#4496=EDGE_CURVE('',#3580,#3582,#1088,.T.);
#4497=EDGE_CURVE('',#3582,#3525,#1089,.T.);
#4498=EDGE_CURVE('',#3550,#3552,#1090,.T.);
#4499=EDGE_CURVE('',#3527,#3583,#1091,.T.);
#4500=EDGE_CURVE('',#3584,#3526,#1092,.T.);
#4501=EDGE_CURVE('',#3584,#3579,#1093,.T.);
#4502=EDGE_CURVE('',#3575,#3583,#1094,.T.);
#4503=EDGE_CURVE('',#3585,#3586,#1095,.T.);
#4504=EDGE_CURVE('',#3585,#3573,#1096,.T.);
#4505=EDGE_CURVE('',#3574,#3586,#1097,.T.);
#4506=EDGE_CURVE('',#3551,#3521,#1098,.T.);
#4507=EDGE_CURVE('',#3582,#3556,#2978,.T.);
#4508=EDGE_CURVE('',#3555,#3584,#2979,.T.);
#4509=EDGE_CURVE('',#3583,#3585,#2980,.T.);
#4510=EDGE_CURVE('',#3586,#3581,#2981,.T.);
#4511=EDGE_CURVE('',#3539,#3562,#1099,.T.);
#4512=EDGE_CURVE('',#3563,#3567,#1100,.T.);
#4513=EDGE_CURVE('',#3566,#3544,#1101,.T.);
#4514=EDGE_CURVE('',#3568,#3565,#1102,.T.);
#4515=EDGE_CURVE('',#3587,#3587,#2982,.T.);
#4516=EDGE_CURVE('',#3587,#3588,#2983,.T.);
#4517=EDGE_CURVE('',#3589,#3589,#2984,.T.);
#4518=EDGE_CURVE('',#3589,#3587,#2985,.T.);
#4519=EDGE_CURVE('',#3590,#3590,#2986,.T.);
#4520=EDGE_CURVE('',#3590,#3591,#1103,.T.);
#4521=EDGE_CURVE('',#3591,#3591,#2987,.T.);
#4522=EDGE_CURVE('',#3592,#3592,#2988,.T.);
#4523=EDGE_CURVE('',#3592,#3593,#1104,.T.);
#4524=EDGE_CURVE('',#3593,#3593,#2989,.T.);
#4525=EDGE_CURVE('',#3594,#3594,#2990,.T.);
#4526=EDGE_CURVE('',#3594,#3595,#1105,.T.);
#4527=EDGE_CURVE('',#3595,#3595,#2991,.T.);
#4528=EDGE_CURVE('',#3596,#3597,#1106,.T.);
#4529=EDGE_CURVE('',#3598,#3596,#1107,.T.);
#4530=EDGE_CURVE('',#3599,#3598,#1108,.T.);
#4531=EDGE_CURVE('',#3597,#3599,#1109,.T.);
#4532=EDGE_CURVE('',#3600,#3601,#2992,.T.);
#4533=EDGE_CURVE('',#3601,#3596,#1110,.T.);
#4534=EDGE_CURVE('',#3600,#3597,#1111,.T.);
#4535=EDGE_CURVE('',#3602,#3599,#1112,.T.);
#4536=EDGE_CURVE('',#3602,#3600,#1113,.T.);
#4537=EDGE_CURVE('',#3603,#3598,#1114,.T.);
#4538=EDGE_CURVE('',#3603,#3602,#2993,.T.);
#4539=EDGE_CURVE('',#3601,#3603,#1115,.T.);
#4540=EDGE_CURVE('',#3604,#3604,#2994,.T.);
#4541=EDGE_CURVE('',#3604,#3605,#1116,.T.);
#4542=EDGE_CURVE('',#3605,#3605,#2995,.T.);
#4543=EDGE_CURVE('',#3606,#3607,#2996,.T.);
#4544=EDGE_CURVE('',#3608,#3606,#1117,.T.);
#4545=EDGE_CURVE('',#3609,#3608,#2997,.T.);
#4546=EDGE_CURVE('',#3607,#3609,#1118,.T.);
#4547=EDGE_CURVE('',#3610,#3610,#2998,.T.);
#4548=EDGE_CURVE('',#3610,#3611,#1119,.T.);
#4549=EDGE_CURVE('',#3611,#3611,#2999,.T.);
#4550=EDGE_CURVE('',#3612,#3613,#1120,.T.);
#4551=EDGE_CURVE('',#3614,#3612,#1121,.T.);
#4552=EDGE_CURVE('',#3615,#3614,#1122,.T.);
#4553=EDGE_CURVE('',#3613,#3615,#1123,.T.);
#4554=EDGE_CURVE('',#3609,#3612,#1124,.T.);
#4555=EDGE_CURVE('',#3608,#3614,#1125,.T.);
#4556=EDGE_CURVE('',#3607,#3613,#1126,.T.);
#4557=EDGE_CURVE('',#3606,#3615,#1127,.T.);
#4558=ORIENTED_EDGE('',*,*,#3616,.F.);
#4559=ORIENTED_EDGE('',*,*,#3617,.F.);
#4560=ORIENTED_EDGE('',*,*,#3618,.F.);
#4561=ORIENTED_EDGE('',*,*,#3619,.T.);
#4562=ORIENTED_EDGE('',*,*,#3620,.F.);
#4563=ORIENTED_EDGE('',*,*,#3621,.F.);
#4564=ORIENTED_EDGE('',*,*,#3622,.F.);
#4565=ORIENTED_EDGE('',*,*,#3623,.F.);
#4566=ORIENTED_EDGE('',*,*,#3624,.F.);
#4567=ORIENTED_EDGE('',*,*,#3625,.T.);
#4568=ORIENTED_EDGE('',*,*,#3626,.F.);
#4569=ORIENTED_EDGE('',*,*,#3627,.T.);
#4570=ORIENTED_EDGE('',*,*,#3628,.T.);
#4571=ORIENTED_EDGE('',*,*,#3629,.T.);
#4572=ORIENTED_EDGE('',*,*,#3628,.F.);
#4573=ORIENTED_EDGE('',*,*,#3630,.T.);
#4574=ORIENTED_EDGE('',*,*,#3631,.T.);
#4575=ORIENTED_EDGE('',*,*,#3632,.T.);
#4576=ORIENTED_EDGE('',*,*,#3631,.F.);
#4577=ORIENTED_EDGE('',*,*,#3633,.T.);
#4578=ORIENTED_EDGE('',*,*,#3634,.T.);
#4579=ORIENTED_EDGE('',*,*,#3635,.T.);
#4580=ORIENTED_EDGE('',*,*,#3636,.F.);
#4581=ORIENTED_EDGE('',*,*,#3637,.F.);
#4582=ORIENTED_EDGE('',*,*,#3638,.T.);
#4583=ORIENTED_EDGE('',*,*,#3639,.T.);
#4584=ORIENTED_EDGE('',*,*,#3640,.F.);
#4585=ORIENTED_EDGE('',*,*,#3641,.F.);
#4586=ORIENTED_EDGE('',*,*,#3642,.T.);
#4587=ORIENTED_EDGE('',*,*,#3643,.T.);
#4588=ORIENTED_EDGE('',*,*,#3644,.T.);
#4589=ORIENTED_EDGE('',*,*,#3645,.T.);
#4590=ORIENTED_EDGE('',*,*,#3646,.T.);
#4591=ORIENTED_EDGE('',*,*,#3637,.T.);
#4592=ORIENTED_EDGE('',*,*,#3647,.F.);
#4593=ORIENTED_EDGE('',*,*,#3629,.F.);
#4594=ORIENTED_EDGE('',*,*,#3648,.F.);
#4595=ORIENTED_EDGE('',*,*,#3649,.T.);
#4596=ORIENTED_EDGE('',*,*,#3641,.T.);
#4597=ORIENTED_EDGE('',*,*,#3650,.F.);
#4598=ORIENTED_EDGE('',*,*,#3651,.F.);
#4599=ORIENTED_EDGE('',*,*,#3652,.T.);
#4600=ORIENTED_EDGE('',*,*,#3648,.T.);
#4601=ORIENTED_EDGE('',*,*,#3653,.F.);
#4602=ORIENTED_EDGE('',*,*,#3639,.F.);
#4603=ORIENTED_EDGE('',*,*,#3654,.T.);
#4604=ORIENTED_EDGE('',*,*,#3655,.F.);
#4605=ORIENTED_EDGE('',*,*,#3656,.F.);
#4606=ORIENTED_EDGE('',*,*,#3627,.F.);
#4607=ORIENTED_EDGE('',*,*,#3657,.T.);
#4608=ORIENTED_EDGE('',*,*,#3658,.T.);
#4609=ORIENTED_EDGE('',*,*,#3659,.T.);
#4610=ORIENTED_EDGE('',*,*,#3660,.T.);
#4611=ORIENTED_EDGE('',*,*,#3661,.T.);
#4612=ORIENTED_EDGE('',*,*,#3662,.F.);
#4613=ORIENTED_EDGE('',*,*,#3663,.F.);
#4614=ORIENTED_EDGE('',*,*,#3664,.F.);
#4615=ORIENTED_EDGE('',*,*,#3665,.F.);
#4616=ORIENTED_EDGE('',*,*,#3666,.F.);
#4617=ORIENTED_EDGE('',*,*,#3667,.T.);
#4618=ORIENTED_EDGE('',*,*,#3668,.F.);
#4619=ORIENTED_EDGE('',*,*,#3669,.T.);
#4620=ORIENTED_EDGE('',*,*,#3618,.T.);
#4621=ORIENTED_EDGE('',*,*,#3636,.T.);
#4622=ORIENTED_EDGE('',*,*,#3620,.T.);
#4623=ORIENTED_EDGE('',*,*,#3647,.T.);
#4624=ORIENTED_EDGE('',*,*,#3640,.T.);
#4625=ORIENTED_EDGE('',*,*,#3653,.T.);
#4626=ORIENTED_EDGE('',*,*,#3650,.T.);
#4627=ORIENTED_EDGE('',*,*,#3670,.T.);
#4628=ORIENTED_EDGE('',*,*,#3671,.T.);
#4629=ORIENTED_EDGE('',*,*,#3672,.T.);
#4630=ORIENTED_EDGE('',*,*,#3673,.T.);
#4631=ORIENTED_EDGE('',*,*,#3674,.T.);
#4632=ORIENTED_EDGE('',*,*,#3675,.T.);
#4633=ORIENTED_EDGE('',*,*,#3676,.T.);
#4634=ORIENTED_EDGE('',*,*,#3677,.T.);
#4635=ORIENTED_EDGE('',*,*,#3678,.T.);
#4636=ORIENTED_EDGE('',*,*,#3679,.T.);
#4637=ORIENTED_EDGE('',*,*,#3680,.T.);
#4638=ORIENTED_EDGE('',*,*,#3681,.T.);
#4639=ORIENTED_EDGE('',*,*,#3682,.T.);
#4640=ORIENTED_EDGE('',*,*,#3683,.T.);
#4641=ORIENTED_EDGE('',*,*,#3684,.T.);
#4642=ORIENTED_EDGE('',*,*,#3685,.T.);
#4643=ORIENTED_EDGE('',*,*,#3686,.T.);
#4644=ORIENTED_EDGE('',*,*,#3687,.T.);
#4645=ORIENTED_EDGE('',*,*,#3616,.T.);
#4646=ORIENTED_EDGE('',*,*,#3688,.F.);
#4647=ORIENTED_EDGE('',*,*,#3689,.T.);
#4648=ORIENTED_EDGE('',*,*,#3690,.T.);
#4649=ORIENTED_EDGE('',*,*,#3691,.T.);
#4650=ORIENTED_EDGE('',*,*,#3692,.T.);
#4651=ORIENTED_EDGE('',*,*,#3693,.F.);
#4652=ORIENTED_EDGE('',*,*,#3622,.T.);
#4653=ORIENTED_EDGE('',*,*,#3694,.T.);
#4654=ORIENTED_EDGE('',*,*,#3695,.T.);
#4655=ORIENTED_EDGE('',*,*,#3696,.T.);
#4656=ORIENTED_EDGE('',*,*,#3697,.T.);
#4657=ORIENTED_EDGE('',*,*,#3698,.T.);
#4658=ORIENTED_EDGE('',*,*,#3699,.T.);
#4659=ORIENTED_EDGE('',*,*,#3700,.T.);
#4660=ORIENTED_EDGE('',*,*,#3701,.T.);
#4661=ORIENTED_EDGE('',*,*,#3702,.T.);
#4662=ORIENTED_EDGE('',*,*,#3667,.F.);
#4663=ORIENTED_EDGE('',*,*,#3703,.F.);
#4664=ORIENTED_EDGE('',*,*,#3704,.F.);
#4665=ORIENTED_EDGE('',*,*,#3661,.F.);
#4666=ORIENTED_EDGE('',*,*,#3630,.F.);
#4667=ORIENTED_EDGE('',*,*,#3705,.F.);
#4668=ORIENTED_EDGE('',*,*,#3706,.T.);
#4669=ORIENTED_EDGE('',*,*,#3707,.F.);
#4670=ORIENTED_EDGE('',*,*,#3663,.T.);
#4671=ORIENTED_EDGE('',*,*,#3708,.F.);
#4672=ORIENTED_EDGE('',*,*,#3709,.T.);
#4673=ORIENTED_EDGE('',*,*,#3665,.T.);
#4674=ORIENTED_EDGE('',*,*,#3632,.F.);
#4675=ORIENTED_EDGE('',*,*,#3702,.F.);
#4676=ORIENTED_EDGE('',*,*,#3710,.T.);
#4677=ORIENTED_EDGE('',*,*,#3705,.T.);
#4678=ORIENTED_EDGE('',*,*,#3668,.T.);
#4679=ORIENTED_EDGE('',*,*,#3707,.T.);
#4680=ORIENTED_EDGE('',*,*,#3711,.T.);
#4681=ORIENTED_EDGE('',*,*,#3700,.F.);
#4682=ORIENTED_EDGE('',*,*,#3664,.T.);
#4683=ORIENTED_EDGE('',*,*,#3706,.F.);
#4684=ORIENTED_EDGE('',*,*,#3710,.F.);
#4685=ORIENTED_EDGE('',*,*,#3701,.F.);
#4686=ORIENTED_EDGE('',*,*,#3711,.F.);
#4687=ORIENTED_EDGE('',*,*,#3666,.T.);
#4688=ORIENTED_EDGE('',*,*,#3709,.F.);
#4689=ORIENTED_EDGE('',*,*,#3712,.F.);
#4690=ORIENTED_EDGE('',*,*,#3703,.T.);
#4691=ORIENTED_EDGE('',*,*,#3662,.T.);
#4692=ORIENTED_EDGE('',*,*,#3704,.T.);
#4693=ORIENTED_EDGE('',*,*,#3712,.T.);
#4694=ORIENTED_EDGE('',*,*,#3708,.T.);
#4695=ORIENTED_EDGE('',*,*,#3713,.F.);
#4696=ORIENTED_EDGE('',*,*,#3697,.F.);
#4697=ORIENTED_EDGE('',*,*,#3714,.F.);
#4698=ORIENTED_EDGE('',*,*,#3680,.F.);
#4699=ORIENTED_EDGE('',*,*,#3715,.F.);
#4700=ORIENTED_EDGE('',*,*,#3713,.T.);
#4701=ORIENTED_EDGE('',*,*,#3716,.F.);
#4702=ORIENTED_EDGE('',*,*,#3717,.F.);
#4703=ORIENTED_EDGE('',*,*,#3714,.T.);
#4704=ORIENTED_EDGE('',*,*,#3718,.F.);
#4705=ORIENTED_EDGE('',*,*,#3716,.T.);
#4706=ORIENTED_EDGE('',*,*,#3679,.F.);
#4707=ORIENTED_EDGE('',*,*,#3719,.F.);
#4708=ORIENTED_EDGE('',*,*,#3677,.F.);
#4709=ORIENTED_EDGE('',*,*,#3715,.T.);
#4710=ORIENTED_EDGE('',*,*,#3676,.F.);
#4711=ORIENTED_EDGE('',*,*,#3720,.F.);
#4712=ORIENTED_EDGE('',*,*,#3698,.F.);
#4713=ORIENTED_EDGE('',*,*,#3718,.T.);
#4714=ORIENTED_EDGE('',*,*,#3696,.F.);
#4715=ORIENTED_EDGE('',*,*,#3625,.F.);
#4716=ORIENTED_EDGE('',*,*,#3684,.F.);
#4717=ORIENTED_EDGE('',*,*,#3717,.T.);
#4718=ORIENTED_EDGE('',*,*,#3683,.F.);
#4719=ORIENTED_EDGE('',*,*,#3721,.F.);
#4720=ORIENTED_EDGE('',*,*,#3681,.F.);
#4721=ORIENTED_EDGE('',*,*,#3722,.F.);
#4722=ORIENTED_EDGE('',*,*,#3678,.F.);
#4723=ORIENTED_EDGE('',*,*,#3723,.F.);
#4724=ORIENTED_EDGE('',*,*,#3691,.F.);
#4725=ORIENTED_EDGE('',*,*,#3719,.T.);
#4726=ORIENTED_EDGE('',*,*,#3722,.T.);
#4727=ORIENTED_EDGE('',*,*,#3724,.F.);
#4728=ORIENTED_EDGE('',*,*,#3725,.F.);
#4729=ORIENTED_EDGE('',*,*,#3720,.T.);
#4730=ORIENTED_EDGE('',*,*,#3726,.F.);
#4731=ORIENTED_EDGE('',*,*,#3723,.T.);
#4732=ORIENTED_EDGE('',*,*,#3721,.T.);
#4733=ORIENTED_EDGE('',*,*,#3727,.F.);
#4734=ORIENTED_EDGE('',*,*,#3724,.T.);
#4735=ORIENTED_EDGE('',*,*,#3690,.F.);
#4736=ORIENTED_EDGE('',*,*,#3728,.F.);
#4737=ORIENTED_EDGE('',*,*,#3674,.F.);
#4738=ORIENTED_EDGE('',*,*,#3726,.T.);
#4739=ORIENTED_EDGE('',*,*,#3675,.F.);
#4740=ORIENTED_EDGE('',*,*,#3729,.F.);
#4741=ORIENTED_EDGE('',*,*,#3673,.F.);
#4742=ORIENTED_EDGE('',*,*,#3725,.T.);
#4743=ORIENTED_EDGE('',*,*,#3672,.F.);
#4744=ORIENTED_EDGE('',*,*,#3730,.F.);
#4745=ORIENTED_EDGE('',*,*,#3699,.F.);
#4746=ORIENTED_EDGE('',*,*,#3621,.T.);
#4747=ORIENTED_EDGE('',*,*,#3635,.F.);
#4748=ORIENTED_EDGE('',*,*,#3731,.F.);
#4749=ORIENTED_EDGE('',*,*,#3694,.F.);
#4750=ORIENTED_EDGE('',*,*,#3626,.T.);
#4751=ORIENTED_EDGE('',*,*,#3695,.F.);
#4752=ORIENTED_EDGE('',*,*,#3732,.F.);
#4753=ORIENTED_EDGE('',*,*,#3659,.F.);
#4754=ORIENTED_EDGE('',*,*,#3624,.T.);
#4755=ORIENTED_EDGE('',*,*,#3658,.F.);
#4756=ORIENTED_EDGE('',*,*,#3733,.F.);
#4757=ORIENTED_EDGE('',*,*,#3685,.F.);
#4758=ORIENTED_EDGE('',*,*,#3727,.T.);
#4759=ORIENTED_EDGE('',*,*,#3682,.F.);
#4760=ORIENTED_EDGE('',*,*,#3734,.F.);
#4761=ORIENTED_EDGE('',*,*,#3692,.F.);
#4762=ORIENTED_EDGE('',*,*,#3729,.T.);
#4763=ORIENTED_EDGE('',*,*,#3728,.T.);
#4764=ORIENTED_EDGE('',*,*,#3735,.F.);
#4765=ORIENTED_EDGE('',*,*,#3693,.T.);
#4766=ORIENTED_EDGE('',*,*,#3730,.T.);
#4767=ORIENTED_EDGE('',*,*,#3736,.F.);
#4768=ORIENTED_EDGE('',*,*,#3623,.T.);
#4769=ORIENTED_EDGE('',*,*,#3732,.T.);
#4770=ORIENTED_EDGE('',*,*,#3731,.T.);
#4771=ORIENTED_EDGE('',*,*,#3737,.F.);
#4772=ORIENTED_EDGE('',*,*,#3734,.T.);
#4773=ORIENTED_EDGE('',*,*,#3733,.T.);
#4774=ORIENTED_EDGE('',*,*,#3738,.F.);
#4775=ORIENTED_EDGE('',*,*,#3735,.T.);
#4776=ORIENTED_EDGE('',*,*,#3689,.F.);
#4777=ORIENTED_EDGE('',*,*,#3739,.F.);
#4778=ORIENTED_EDGE('',*,*,#3670,.F.);
#4779=ORIENTED_EDGE('',*,*,#3736,.T.);
#4780=ORIENTED_EDGE('',*,*,#3671,.F.);
#4781=ORIENTED_EDGE('',*,*,#3740,.F.);
#4782=ORIENTED_EDGE('',*,*,#3669,.F.);
#4783=ORIENTED_EDGE('',*,*,#3737,.T.);
#4784=ORIENTED_EDGE('',*,*,#3634,.F.);
#4785=ORIENTED_EDGE('',*,*,#3741,.F.);
#4786=ORIENTED_EDGE('',*,*,#3660,.F.);
#4787=ORIENTED_EDGE('',*,*,#3738,.T.);
#4788=ORIENTED_EDGE('',*,*,#3657,.F.);
#4789=ORIENTED_EDGE('',*,*,#3742,.F.);
#4790=ORIENTED_EDGE('',*,*,#3686,.F.);
#4791=ORIENTED_EDGE('',*,*,#3739,.T.);
#4792=ORIENTED_EDGE('',*,*,#3688,.T.);
#4793=ORIENTED_EDGE('',*,*,#3619,.F.);
#4794=ORIENTED_EDGE('',*,*,#3740,.T.);
#4795=ORIENTED_EDGE('',*,*,#3742,.T.);
#4796=ORIENTED_EDGE('',*,*,#3741,.T.);
#4797=ORIENTED_EDGE('',*,*,#3743,.F.);
#4798=ORIENTED_EDGE('',*,*,#3743,.T.);
#4799=ORIENTED_EDGE('',*,*,#3633,.F.);
#4800=ORIENTED_EDGE('',*,*,#3617,.T.);
#4801=ORIENTED_EDGE('',*,*,#3687,.F.);
#4802=ORIENTED_EDGE('',*,*,#3656,.T.);
#4803=ORIENTED_EDGE('',*,*,#3744,.T.);
#4804=ORIENTED_EDGE('',*,*,#3644,.F.);
#4805=ORIENTED_EDGE('',*,*,#3745,.F.);
#4806=ORIENTED_EDGE('',*,*,#3655,.T.);
#4807=ORIENTED_EDGE('',*,*,#3746,.T.);
#4808=ORIENTED_EDGE('',*,*,#3645,.F.);
#4809=ORIENTED_EDGE('',*,*,#3744,.F.);
#4810=ORIENTED_EDGE('',*,*,#3643,.F.);
#4811=ORIENTED_EDGE('',*,*,#3747,.T.);
#4812=ORIENTED_EDGE('',*,*,#3651,.T.);
#4813=ORIENTED_EDGE('',*,*,#3745,.T.);
#4814=ORIENTED_EDGE('',*,*,#3652,.F.);
#4815=ORIENTED_EDGE('',*,*,#3747,.F.);
#4816=ORIENTED_EDGE('',*,*,#3642,.F.);
#4817=ORIENTED_EDGE('',*,*,#3649,.F.);
#4818=ORIENTED_EDGE('',*,*,#3654,.F.);
#4819=ORIENTED_EDGE('',*,*,#3638,.F.);
#4820=ORIENTED_EDGE('',*,*,#3646,.F.);
#4821=ORIENTED_EDGE('',*,*,#3746,.F.);
#4822=ORIENTED_EDGE('',*,*,#3748,.T.);
#4823=ORIENTED_EDGE('',*,*,#3749,.F.);
#4824=ORIENTED_EDGE('',*,*,#3750,.F.);
#4825=ORIENTED_EDGE('',*,*,#3751,.F.);
#4826=ORIENTED_EDGE('',*,*,#3752,.T.);
#4827=ORIENTED_EDGE('',*,*,#3753,.F.);
#4828=ORIENTED_EDGE('',*,*,#3754,.F.);
#4829=ORIENTED_EDGE('',*,*,#3755,.F.);
#4830=ORIENTED_EDGE('',*,*,#3756,.F.);
#4831=ORIENTED_EDGE('',*,*,#3757,.F.);
#4832=ORIENTED_EDGE('',*,*,#3758,.T.);
#4833=ORIENTED_EDGE('',*,*,#3759,.T.);
#4834=ORIENTED_EDGE('',*,*,#3760,.T.);
#4835=ORIENTED_EDGE('',*,*,#3759,.F.);
#4836=ORIENTED_EDGE('',*,*,#3761,.T.);
#4837=ORIENTED_EDGE('',*,*,#3762,.T.);
#4838=ORIENTED_EDGE('',*,*,#3763,.T.);
#4839=ORIENTED_EDGE('',*,*,#3762,.F.);
#4840=ORIENTED_EDGE('',*,*,#3764,.T.);
#4841=ORIENTED_EDGE('',*,*,#3765,.T.);
#4842=ORIENTED_EDGE('',*,*,#3766,.F.);
#4843=ORIENTED_EDGE('',*,*,#3765,.F.);
#4844=ORIENTED_EDGE('',*,*,#3767,.T.);
#4845=ORIENTED_EDGE('',*,*,#3768,.T.);
#4846=ORIENTED_EDGE('',*,*,#3769,.T.);
#4847=ORIENTED_EDGE('',*,*,#3768,.F.);
#4848=ORIENTED_EDGE('',*,*,#3770,.F.);
#4849=ORIENTED_EDGE('',*,*,#3771,.T.);
#4850=ORIENTED_EDGE('',*,*,#3772,.T.);
#4851=ORIENTED_EDGE('',*,*,#3773,.T.);
#4852=ORIENTED_EDGE('',*,*,#3771,.F.);
#4853=ORIENTED_EDGE('',*,*,#3774,.T.);
#4854=ORIENTED_EDGE('',*,*,#3775,.T.);
#4855=ORIENTED_EDGE('',*,*,#3776,.F.);
#4856=ORIENTED_EDGE('',*,*,#3775,.F.);
#4857=ORIENTED_EDGE('',*,*,#3777,.T.);
#4858=ORIENTED_EDGE('',*,*,#3778,.F.);
#4859=ORIENTED_EDGE('',*,*,#3779,.F.);
#4860=ORIENTED_EDGE('',*,*,#3780,.F.);
#4861=ORIENTED_EDGE('',*,*,#3781,.T.);
#4862=ORIENTED_EDGE('',*,*,#3782,.T.);
#4863=ORIENTED_EDGE('',*,*,#3783,.T.);
#4864=ORIENTED_EDGE('',*,*,#3784,.T.);
#4865=ORIENTED_EDGE('',*,*,#3785,.T.);
#4866=ORIENTED_EDGE('',*,*,#3783,.F.);
#4867=ORIENTED_EDGE('',*,*,#3786,.T.);
#4868=ORIENTED_EDGE('',*,*,#3787,.T.);
#4869=ORIENTED_EDGE('',*,*,#3788,.F.);
#4870=ORIENTED_EDGE('',*,*,#3789,.F.);
#4871=ORIENTED_EDGE('',*,*,#3774,.F.);
#4872=ORIENTED_EDGE('',*,*,#3777,.F.);
#4873=ORIENTED_EDGE('',*,*,#3773,.F.);
#4874=ORIENTED_EDGE('',*,*,#3772,.F.);
#4875=ORIENTED_EDGE('',*,*,#3790,.T.);
#4876=ORIENTED_EDGE('',*,*,#3749,.T.);
#4877=ORIENTED_EDGE('',*,*,#3791,.T.);
#4878=ORIENTED_EDGE('',*,*,#3792,.F.);
#4879=ORIENTED_EDGE('',*,*,#3750,.T.);
#4880=ORIENTED_EDGE('',*,*,#3790,.F.);
#4881=ORIENTED_EDGE('',*,*,#3793,.T.);
#4882=ORIENTED_EDGE('',*,*,#3794,.T.);
#4883=ORIENTED_EDGE('',*,*,#3756,.T.);
#4884=ORIENTED_EDGE('',*,*,#3795,.F.);
#4885=ORIENTED_EDGE('',*,*,#3796,.T.);
#4886=ORIENTED_EDGE('',*,*,#3797,.T.);
#4887=ORIENTED_EDGE('',*,*,#3798,.T.);
#4888=ORIENTED_EDGE('',*,*,#3799,.F.);
#4889=ORIENTED_EDGE('',*,*,#3800,.T.);
#4890=ORIENTED_EDGE('',*,*,#3801,.T.);
#4891=ORIENTED_EDGE('',*,*,#3802,.F.);
#4892=ORIENTED_EDGE('',*,*,#3803,.F.);
#4893=ORIENTED_EDGE('',*,*,#3804,.T.);
#4894=ORIENTED_EDGE('',*,*,#3788,.T.);
#4895=ORIENTED_EDGE('',*,*,#3802,.T.);
#4896=ORIENTED_EDGE('',*,*,#3780,.T.);
#4897=ORIENTED_EDGE('',*,*,#3805,.T.);
#4898=ORIENTED_EDGE('',*,*,#3785,.F.);
#4899=ORIENTED_EDGE('',*,*,#3784,.F.);
#4900=ORIENTED_EDGE('',*,*,#3806,.F.);
#4901=ORIENTED_EDGE('',*,*,#3807,.F.);
#4902=ORIENTED_EDGE('',*,*,#3808,.F.);
#4903=ORIENTED_EDGE('',*,*,#3809,.F.);
#4904=ORIENTED_EDGE('',*,*,#3778,.T.);
#4905=ORIENTED_EDGE('',*,*,#3810,.T.);
#4906=ORIENTED_EDGE('',*,*,#3811,.F.);
#4907=ORIENTED_EDGE('',*,*,#3812,.F.);
#4908=ORIENTED_EDGE('',*,*,#3789,.T.);
#4909=ORIENTED_EDGE('',*,*,#3804,.F.);
#4910=ORIENTED_EDGE('',*,*,#3813,.F.);
#4911=ORIENTED_EDGE('',*,*,#3810,.F.);
#4912=ORIENTED_EDGE('',*,*,#3770,.T.);
#4913=ORIENTED_EDGE('',*,*,#3779,.T.);
#4914=ORIENTED_EDGE('',*,*,#3812,.T.);
#4915=ORIENTED_EDGE('',*,*,#3814,.F.);
#4916=ORIENTED_EDGE('',*,*,#3805,.F.);
#4917=ORIENTED_EDGE('',*,*,#3776,.T.);
#4918=ORIENTED_EDGE('',*,*,#3803,.T.);
#4919=ORIENTED_EDGE('',*,*,#3814,.T.);
#4920=ORIENTED_EDGE('',*,*,#3811,.T.);
#4921=ORIENTED_EDGE('',*,*,#3813,.T.);
#4922=ORIENTED_EDGE('',*,*,#3801,.F.);
#4923=ORIENTED_EDGE('',*,*,#3815,.T.);
#4924=ORIENTED_EDGE('',*,*,#3816,.T.);
#4925=ORIENTED_EDGE('',*,*,#3817,.F.);
#4926=ORIENTED_EDGE('',*,*,#3818,.F.);
#4927=ORIENTED_EDGE('',*,*,#3819,.T.);
#4928=ORIENTED_EDGE('',*,*,#3820,.T.);
#4929=ORIENTED_EDGE('',*,*,#3821,.F.);
#4930=ORIENTED_EDGE('',*,*,#3781,.F.);
#4931=ORIENTED_EDGE('',*,*,#3817,.T.);
#4932=ORIENTED_EDGE('',*,*,#3822,.F.);
#4933=ORIENTED_EDGE('',*,*,#3823,.T.);
#4934=ORIENTED_EDGE('',*,*,#3763,.F.);
#4935=ORIENTED_EDGE('',*,*,#3782,.F.);
#4936=ORIENTED_EDGE('',*,*,#3821,.T.);
#4937=ORIENTED_EDGE('',*,*,#3824,.T.);
#4938=ORIENTED_EDGE('',*,*,#3825,.F.);
#4939=ORIENTED_EDGE('',*,*,#3786,.F.);
#4940=ORIENTED_EDGE('',*,*,#3826,.F.);
#4941=ORIENTED_EDGE('',*,*,#3827,.T.);
#4942=ORIENTED_EDGE('',*,*,#3797,.F.);
#4943=ORIENTED_EDGE('',*,*,#3828,.T.);
#4944=ORIENTED_EDGE('',*,*,#3829,.T.);
#4945=ORIENTED_EDGE('',*,*,#3815,.F.);
#4946=ORIENTED_EDGE('',*,*,#3787,.F.);
#4947=ORIENTED_EDGE('',*,*,#3825,.T.);
#4948=ORIENTED_EDGE('',*,*,#3764,.F.);
#4949=ORIENTED_EDGE('',*,*,#3795,.T.);
#4950=ORIENTED_EDGE('',*,*,#3755,.T.);
#4951=ORIENTED_EDGE('',*,*,#3830,.T.);
#4952=ORIENTED_EDGE('',*,*,#3831,.T.);
#4953=ORIENTED_EDGE('',*,*,#3822,.T.);
#4954=ORIENTED_EDGE('',*,*,#3816,.F.);
#4955=ORIENTED_EDGE('',*,*,#3829,.F.);
#4956=ORIENTED_EDGE('',*,*,#3832,.T.);
#4957=ORIENTED_EDGE('',*,*,#3833,.T.);
#4958=ORIENTED_EDGE('',*,*,#3751,.T.);
#4959=ORIENTED_EDGE('',*,*,#3792,.T.);
#4960=ORIENTED_EDGE('',*,*,#3834,.T.);
#4961=ORIENTED_EDGE('',*,*,#3835,.F.);
#4962=ORIENTED_EDGE('',*,*,#3753,.T.);
#4963=ORIENTED_EDGE('',*,*,#3836,.F.);
#4964=ORIENTED_EDGE('',*,*,#3837,.T.);
#4965=ORIENTED_EDGE('',*,*,#3826,.T.);
#4966=ORIENTED_EDGE('',*,*,#3824,.F.);
#4967=ORIENTED_EDGE('',*,*,#3820,.F.);
#4968=ORIENTED_EDGE('',*,*,#3838,.T.);
#4969=ORIENTED_EDGE('',*,*,#3839,.F.);
#4970=ORIENTED_EDGE('',*,*,#3840,.T.);
#4971=ORIENTED_EDGE('',*,*,#3818,.T.);
#4972=ORIENTED_EDGE('',*,*,#3841,.T.);
#4973=ORIENTED_EDGE('',*,*,#3842,.T.);
#4974=ORIENTED_EDGE('',*,*,#3757,.T.);
#4975=ORIENTED_EDGE('',*,*,#3794,.F.);
#4976=ORIENTED_EDGE('',*,*,#3836,.T.);
#4977=ORIENTED_EDGE('',*,*,#3752,.F.);
#4978=ORIENTED_EDGE('',*,*,#3833,.F.);
#4979=ORIENTED_EDGE('',*,*,#3843,.T.);
#4980=ORIENTED_EDGE('',*,*,#3799,.T.);
#4981=ORIENTED_EDGE('',*,*,#3844,.T.);
#4982=ORIENTED_EDGE('',*,*,#3769,.F.);
#4983=ORIENTED_EDGE('',*,*,#3830,.F.);
#4984=ORIENTED_EDGE('',*,*,#3754,.T.);
#4985=ORIENTED_EDGE('',*,*,#3835,.T.);
#4986=ORIENTED_EDGE('',*,*,#3845,.T.);
#4987=ORIENTED_EDGE('',*,*,#3839,.T.);
#4988=ORIENTED_EDGE('',*,*,#3846,.T.);
#4989=ORIENTED_EDGE('',*,*,#3767,.F.);
#4990=ORIENTED_EDGE('',*,*,#3766,.T.);
#4991=ORIENTED_EDGE('',*,*,#3761,.F.);
#4992=ORIENTED_EDGE('',*,*,#3845,.F.);
#4993=ORIENTED_EDGE('',*,*,#3838,.F.);
#4994=ORIENTED_EDGE('',*,*,#3819,.F.);
#4995=ORIENTED_EDGE('',*,*,#3840,.F.);
#4996=ORIENTED_EDGE('',*,*,#3827,.F.);
#4997=ORIENTED_EDGE('',*,*,#3837,.F.);
#4998=ORIENTED_EDGE('',*,*,#3844,.F.);
#4999=ORIENTED_EDGE('',*,*,#3798,.F.);
#5000=ORIENTED_EDGE('',*,*,#3843,.F.);
#5001=ORIENTED_EDGE('',*,*,#3832,.F.);
#5002=ORIENTED_EDGE('',*,*,#3828,.F.);
#5003=ORIENTED_EDGE('',*,*,#3800,.F.);
#5004=ORIENTED_EDGE('',*,*,#3823,.F.);
#5005=ORIENTED_EDGE('',*,*,#3831,.F.);
#5006=ORIENTED_EDGE('',*,*,#3846,.F.);
#5007=ORIENTED_EDGE('',*,*,#3841,.F.);
#5008=ORIENTED_EDGE('',*,*,#3748,.F.);
#5009=ORIENTED_EDGE('',*,*,#3842,.F.);
#5010=ORIENTED_EDGE('',*,*,#3796,.F.);
#5011=ORIENTED_EDGE('',*,*,#3834,.F.);
#5012=ORIENTED_EDGE('',*,*,#3793,.F.);
#5013=ORIENTED_EDGE('',*,*,#3791,.F.);
#5014=ORIENTED_EDGE('',*,*,#3847,.T.);
#5015=ORIENTED_EDGE('',*,*,#3848,.T.);
#5016=ORIENTED_EDGE('',*,*,#3849,.T.);
#5017=ORIENTED_EDGE('',*,*,#3850,.T.);
#5018=ORIENTED_EDGE('',*,*,#3851,.T.);
#5019=ORIENTED_EDGE('',*,*,#3852,.T.);
#5020=ORIENTED_EDGE('',*,*,#3847,.F.);
#5021=ORIENTED_EDGE('',*,*,#3853,.T.);
#5022=ORIENTED_EDGE('',*,*,#3854,.F.);
#5023=ORIENTED_EDGE('',*,*,#3807,.T.);
#5024=ORIENTED_EDGE('',*,*,#3760,.F.);
#5025=ORIENTED_EDGE('',*,*,#3855,.T.);
#5026=ORIENTED_EDGE('',*,*,#3856,.T.);
#5027=ORIENTED_EDGE('',*,*,#3851,.F.);
#5028=ORIENTED_EDGE('',*,*,#3806,.T.);
#5029=ORIENTED_EDGE('',*,*,#3849,.F.);
#5030=ORIENTED_EDGE('',*,*,#3857,.T.);
#5031=ORIENTED_EDGE('',*,*,#3855,.F.);
#5032=ORIENTED_EDGE('',*,*,#3809,.T.);
#5033=ORIENTED_EDGE('',*,*,#3858,.T.);
#5034=ORIENTED_EDGE('',*,*,#3859,.T.);
#5035=ORIENTED_EDGE('',*,*,#3758,.F.);
#5036=ORIENTED_EDGE('',*,*,#3854,.T.);
#5037=ORIENTED_EDGE('',*,*,#3860,.T.);
#5038=ORIENTED_EDGE('',*,*,#3858,.F.);
#5039=ORIENTED_EDGE('',*,*,#3808,.T.);
#5040=ORIENTED_EDGE('',*,*,#3852,.F.);
#5041=ORIENTED_EDGE('',*,*,#3856,.F.);
#5042=ORIENTED_EDGE('',*,*,#3857,.F.);
#5043=ORIENTED_EDGE('',*,*,#3848,.F.);
#5044=ORIENTED_EDGE('',*,*,#3859,.F.);
#5045=ORIENTED_EDGE('',*,*,#3860,.F.);
#5046=ORIENTED_EDGE('',*,*,#3853,.F.);
#5047=ORIENTED_EDGE('',*,*,#3850,.F.);
#5048=ORIENTED_EDGE('',*,*,#3861,.T.);
#5049=ORIENTED_EDGE('',*,*,#3862,.T.);
#5050=ORIENTED_EDGE('',*,*,#3863,.T.);
#5051=ORIENTED_EDGE('',*,*,#3862,.F.);
#5052=ORIENTED_EDGE('',*,*,#3864,.T.);
#5053=ORIENTED_EDGE('',*,*,#3865,.T.);
#5054=ORIENTED_EDGE('',*,*,#3866,.T.);
#5055=ORIENTED_EDGE('',*,*,#3865,.F.);
#5056=ORIENTED_EDGE('',*,*,#3867,.T.);
#5057=ORIENTED_EDGE('',*,*,#3868,.T.);
#5058=ORIENTED_EDGE('',*,*,#3869,.F.);
#5059=ORIENTED_EDGE('',*,*,#3868,.F.);
#5060=ORIENTED_EDGE('',*,*,#3870,.T.);
#5061=ORIENTED_EDGE('',*,*,#3871,.T.);
#5062=ORIENTED_EDGE('',*,*,#3872,.T.);
#5063=ORIENTED_EDGE('',*,*,#3871,.F.);
#5064=ORIENTED_EDGE('',*,*,#3873,.F.);
#5065=ORIENTED_EDGE('',*,*,#3874,.T.);
#5066=ORIENTED_EDGE('',*,*,#3875,.T.);
#5067=ORIENTED_EDGE('',*,*,#3876,.T.);
#5068=ORIENTED_EDGE('',*,*,#3874,.F.);
#5069=ORIENTED_EDGE('',*,*,#3877,.T.);
#5070=ORIENTED_EDGE('',*,*,#3878,.T.);
#5071=ORIENTED_EDGE('',*,*,#3879,.F.);
#5072=ORIENTED_EDGE('',*,*,#3878,.F.);
#5073=ORIENTED_EDGE('',*,*,#3880,.T.);
#5074=ORIENTED_EDGE('',*,*,#3881,.T.);
#5075=ORIENTED_EDGE('',*,*,#3882,.F.);
#5076=ORIENTED_EDGE('',*,*,#3883,.F.);
#5077=ORIENTED_EDGE('',*,*,#3884,.T.);
#5078=ORIENTED_EDGE('',*,*,#3885,.F.);
#5079=ORIENTED_EDGE('',*,*,#3886,.T.);
#5080=ORIENTED_EDGE('',*,*,#3887,.T.);
#5081=ORIENTED_EDGE('',*,*,#3888,.T.);
#5082=ORIENTED_EDGE('',*,*,#3889,.T.);
#5083=ORIENTED_EDGE('',*,*,#3890,.T.);
#5084=ORIENTED_EDGE('',*,*,#3888,.F.);
#5085=ORIENTED_EDGE('',*,*,#3891,.T.);
#5086=ORIENTED_EDGE('',*,*,#3892,.T.);
#5087=ORIENTED_EDGE('',*,*,#3893,.F.);
#5088=ORIENTED_EDGE('',*,*,#3894,.T.);
#5089=ORIENTED_EDGE('',*,*,#3895,.F.);
#5090=ORIENTED_EDGE('',*,*,#3896,.F.);
#5091=ORIENTED_EDGE('',*,*,#3877,.F.);
#5092=ORIENTED_EDGE('',*,*,#3880,.F.);
#5093=ORIENTED_EDGE('',*,*,#3876,.F.);
#5094=ORIENTED_EDGE('',*,*,#3875,.F.);
#5095=ORIENTED_EDGE('',*,*,#3897,.T.);
#5096=ORIENTED_EDGE('',*,*,#3898,.T.);
#5097=ORIENTED_EDGE('',*,*,#3893,.T.);
#5098=ORIENTED_EDGE('',*,*,#3899,.T.);
#5099=ORIENTED_EDGE('',*,*,#3885,.T.);
#5100=ORIENTED_EDGE('',*,*,#3900,.T.);
#5101=ORIENTED_EDGE('',*,*,#3901,.T.);
#5102=ORIENTED_EDGE('',*,*,#3902,.F.);
#5103=ORIENTED_EDGE('',*,*,#3903,.T.);
#5104=ORIENTED_EDGE('',*,*,#3904,.T.);
#5105=ORIENTED_EDGE('',*,*,#3905,.F.);
#5106=ORIENTED_EDGE('',*,*,#3906,.T.);
#5107=ORIENTED_EDGE('',*,*,#3907,.T.);
#5108=ORIENTED_EDGE('',*,*,#3899,.F.);
#5109=ORIENTED_EDGE('',*,*,#3890,.F.);
#5110=ORIENTED_EDGE('',*,*,#3889,.F.);
#5111=ORIENTED_EDGE('',*,*,#3908,.F.);
#5112=ORIENTED_EDGE('',*,*,#3909,.F.);
#5113=ORIENTED_EDGE('',*,*,#3910,.F.);
#5114=ORIENTED_EDGE('',*,*,#3911,.F.);
#5115=ORIENTED_EDGE('',*,*,#3912,.T.);
#5116=ORIENTED_EDGE('',*,*,#3913,.T.);
#5117=ORIENTED_EDGE('',*,*,#3914,.F.);
#5118=ORIENTED_EDGE('',*,*,#3915,.F.);
#5119=ORIENTED_EDGE('',*,*,#3916,.T.);
#5120=ORIENTED_EDGE('',*,*,#3917,.T.);
#5121=ORIENTED_EDGE('',*,*,#3897,.F.);
#5122=ORIENTED_EDGE('',*,*,#3918,.F.);
#5123=ORIENTED_EDGE('',*,*,#3913,.F.);
#5124=ORIENTED_EDGE('',*,*,#3919,.T.);
#5125=ORIENTED_EDGE('',*,*,#3896,.T.);
#5126=ORIENTED_EDGE('',*,*,#3873,.T.);
#5127=ORIENTED_EDGE('',*,*,#3901,.F.);
#5128=ORIENTED_EDGE('',*,*,#3920,.T.);
#5129=ORIENTED_EDGE('',*,*,#3921,.T.);
#5130=ORIENTED_EDGE('',*,*,#3882,.T.);
#5131=ORIENTED_EDGE('',*,*,#3922,.T.);
#5132=ORIENTED_EDGE('',*,*,#3915,.T.);
#5133=ORIENTED_EDGE('',*,*,#3923,.F.);
#5134=ORIENTED_EDGE('',*,*,#3879,.T.);
#5135=ORIENTED_EDGE('',*,*,#3902,.T.);
#5136=ORIENTED_EDGE('',*,*,#3923,.T.);
#5137=ORIENTED_EDGE('',*,*,#3914,.T.);
#5138=ORIENTED_EDGE('',*,*,#3918,.T.);
#5139=ORIENTED_EDGE('',*,*,#3907,.F.);
#5140=ORIENTED_EDGE('',*,*,#3924,.T.);
#5141=ORIENTED_EDGE('',*,*,#3925,.T.);
#5142=ORIENTED_EDGE('',*,*,#3926,.F.);
#5143=ORIENTED_EDGE('',*,*,#3927,.F.);
#5144=ORIENTED_EDGE('',*,*,#3928,.T.);
#5145=ORIENTED_EDGE('',*,*,#3929,.T.);
#5146=ORIENTED_EDGE('',*,*,#3930,.F.);
#5147=ORIENTED_EDGE('',*,*,#3886,.F.);
#5148=ORIENTED_EDGE('',*,*,#3926,.T.);
#5149=ORIENTED_EDGE('',*,*,#3931,.F.);
#5150=ORIENTED_EDGE('',*,*,#3932,.T.);
#5151=ORIENTED_EDGE('',*,*,#3866,.F.);
#5152=ORIENTED_EDGE('',*,*,#3887,.F.);
#5153=ORIENTED_EDGE('',*,*,#3930,.T.);
#5154=ORIENTED_EDGE('',*,*,#3933,.T.);
#5155=ORIENTED_EDGE('',*,*,#3934,.F.);
#5156=ORIENTED_EDGE('',*,*,#3891,.F.);
#5157=ORIENTED_EDGE('',*,*,#3935,.F.);
#5158=ORIENTED_EDGE('',*,*,#3936,.T.);
#5159=ORIENTED_EDGE('',*,*,#3903,.F.);
#5160=ORIENTED_EDGE('',*,*,#3937,.T.);
#5161=ORIENTED_EDGE('',*,*,#3938,.T.);
#5162=ORIENTED_EDGE('',*,*,#3924,.F.);
#5163=ORIENTED_EDGE('',*,*,#3892,.F.);
#5164=ORIENTED_EDGE('',*,*,#3934,.T.);
#5165=ORIENTED_EDGE('',*,*,#3867,.F.);
#5166=ORIENTED_EDGE('',*,*,#3938,.F.);
#5167=ORIENTED_EDGE('',*,*,#3939,.T.);
#5168=ORIENTED_EDGE('',*,*,#3940,.T.);
#5169=ORIENTED_EDGE('',*,*,#3941,.T.);
#5170=ORIENTED_EDGE('',*,*,#3942,.T.);
#5171=ORIENTED_EDGE('',*,*,#3943,.T.);
#5172=ORIENTED_EDGE('',*,*,#3931,.T.);
#5173=ORIENTED_EDGE('',*,*,#3925,.F.);
#5174=ORIENTED_EDGE('',*,*,#3944,.F.);
#5175=ORIENTED_EDGE('',*,*,#3945,.T.);
#5176=ORIENTED_EDGE('',*,*,#3946,.F.);
#5177=ORIENTED_EDGE('',*,*,#3947,.T.);
#5178=ORIENTED_EDGE('',*,*,#3935,.T.);
#5179=ORIENTED_EDGE('',*,*,#3933,.F.);
#5180=ORIENTED_EDGE('',*,*,#3929,.F.);
#5181=ORIENTED_EDGE('',*,*,#3948,.T.);
#5182=ORIENTED_EDGE('',*,*,#3949,.F.);
#5183=ORIENTED_EDGE('',*,*,#3950,.T.);
#5184=ORIENTED_EDGE('',*,*,#3927,.T.);
#5185=ORIENTED_EDGE('',*,*,#3951,.T.);
#5186=ORIENTED_EDGE('',*,*,#3952,.T.);
#5187=ORIENTED_EDGE('',*,*,#3953,.T.);
#5188=ORIENTED_EDGE('',*,*,#3954,.F.);
#5189=ORIENTED_EDGE('',*,*,#3955,.T.);
#5190=ORIENTED_EDGE('',*,*,#3905,.T.);
#5191=ORIENTED_EDGE('',*,*,#3956,.T.);
#5192=ORIENTED_EDGE('',*,*,#3946,.T.);
#5193=ORIENTED_EDGE('',*,*,#3957,.T.);
#5194=ORIENTED_EDGE('',*,*,#3952,.F.);
#5195=ORIENTED_EDGE('',*,*,#3958,.T.);
#5196=ORIENTED_EDGE('',*,*,#3940,.F.);
#5197=ORIENTED_EDGE('',*,*,#3959,.T.);
#5198=ORIENTED_EDGE('',*,*,#3872,.F.);
#5199=ORIENTED_EDGE('',*,*,#3944,.T.);
#5200=ORIENTED_EDGE('',*,*,#3960,.T.);
#5201=ORIENTED_EDGE('',*,*,#3949,.T.);
#5202=ORIENTED_EDGE('',*,*,#3961,.T.);
#5203=ORIENTED_EDGE('',*,*,#3942,.F.);
#5204=ORIENTED_EDGE('',*,*,#3962,.T.);
#5205=ORIENTED_EDGE('',*,*,#3954,.T.);
#5206=ORIENTED_EDGE('',*,*,#3963,.T.);
#5207=ORIENTED_EDGE('',*,*,#3870,.F.);
#5208=ORIENTED_EDGE('',*,*,#3869,.T.);
#5209=ORIENTED_EDGE('',*,*,#3864,.F.);
#5210=ORIENTED_EDGE('',*,*,#3957,.F.);
#5211=ORIENTED_EDGE('',*,*,#3945,.F.);
#5212=ORIENTED_EDGE('',*,*,#3963,.F.);
#5213=ORIENTED_EDGE('',*,*,#3953,.F.);
#5214=ORIENTED_EDGE('',*,*,#3960,.F.);
#5215=ORIENTED_EDGE('',*,*,#3948,.F.);
#5216=ORIENTED_EDGE('',*,*,#3928,.F.);
#5217=ORIENTED_EDGE('',*,*,#3950,.F.);
#5218=ORIENTED_EDGE('',*,*,#3936,.F.);
#5219=ORIENTED_EDGE('',*,*,#3947,.F.);
#5220=ORIENTED_EDGE('',*,*,#3956,.F.);
#5221=ORIENTED_EDGE('',*,*,#3904,.F.);
#5222=ORIENTED_EDGE('',*,*,#3959,.F.);
#5223=ORIENTED_EDGE('',*,*,#3939,.F.);
#5224=ORIENTED_EDGE('',*,*,#3937,.F.);
#5225=ORIENTED_EDGE('',*,*,#3906,.F.);
#5226=ORIENTED_EDGE('',*,*,#3932,.F.);
#5227=ORIENTED_EDGE('',*,*,#3943,.F.);
#5228=ORIENTED_EDGE('',*,*,#3961,.F.);
#5229=ORIENTED_EDGE('',*,*,#3951,.F.);
#5230=ORIENTED_EDGE('',*,*,#3958,.F.);
#5231=ORIENTED_EDGE('',*,*,#3955,.F.);
#5232=ORIENTED_EDGE('',*,*,#3962,.F.);
#5233=ORIENTED_EDGE('',*,*,#3941,.F.);
#5234=ORIENTED_EDGE('',*,*,#3964,.T.);
#5235=ORIENTED_EDGE('',*,*,#3965,.T.);
#5236=ORIENTED_EDGE('',*,*,#3966,.T.);
#5237=ORIENTED_EDGE('',*,*,#3967,.T.);
#5238=ORIENTED_EDGE('',*,*,#3968,.T.);
#5239=ORIENTED_EDGE('',*,*,#3969,.T.);
#5240=ORIENTED_EDGE('',*,*,#3964,.F.);
#5241=ORIENTED_EDGE('',*,*,#3970,.T.);
#5242=ORIENTED_EDGE('',*,*,#3971,.F.);
#5243=ORIENTED_EDGE('',*,*,#3909,.T.);
#5244=ORIENTED_EDGE('',*,*,#3863,.F.);
#5245=ORIENTED_EDGE('',*,*,#3972,.T.);
#5246=ORIENTED_EDGE('',*,*,#3973,.T.);
#5247=ORIENTED_EDGE('',*,*,#3968,.F.);
#5248=ORIENTED_EDGE('',*,*,#3908,.T.);
#5249=ORIENTED_EDGE('',*,*,#3966,.F.);
#5250=ORIENTED_EDGE('',*,*,#3974,.T.);
#5251=ORIENTED_EDGE('',*,*,#3972,.F.);
#5252=ORIENTED_EDGE('',*,*,#3911,.T.);
#5253=ORIENTED_EDGE('',*,*,#3975,.T.);
#5254=ORIENTED_EDGE('',*,*,#3976,.T.);
#5255=ORIENTED_EDGE('',*,*,#3861,.F.);
#5256=ORIENTED_EDGE('',*,*,#3971,.T.);
#5257=ORIENTED_EDGE('',*,*,#3977,.T.);
#5258=ORIENTED_EDGE('',*,*,#3975,.F.);
#5259=ORIENTED_EDGE('',*,*,#3910,.T.);
#5260=ORIENTED_EDGE('',*,*,#3969,.F.);
#5261=ORIENTED_EDGE('',*,*,#3973,.F.);
#5262=ORIENTED_EDGE('',*,*,#3974,.F.);
#5263=ORIENTED_EDGE('',*,*,#3965,.F.);
#5264=ORIENTED_EDGE('',*,*,#3976,.F.);
#5265=ORIENTED_EDGE('',*,*,#3977,.F.);
#5266=ORIENTED_EDGE('',*,*,#3970,.F.);
#5267=ORIENTED_EDGE('',*,*,#3967,.F.);
#5268=ORIENTED_EDGE('',*,*,#3921,.F.);
#5269=ORIENTED_EDGE('',*,*,#3978,.T.);
#5270=ORIENTED_EDGE('',*,*,#3883,.T.);
#5271=ORIENTED_EDGE('',*,*,#3895,.T.);
#5272=ORIENTED_EDGE('',*,*,#3979,.T.);
#5273=ORIENTED_EDGE('',*,*,#3916,.F.);
#5274=ORIENTED_EDGE('',*,*,#3917,.F.);
#5275=ORIENTED_EDGE('',*,*,#3979,.F.);
#5276=ORIENTED_EDGE('',*,*,#3894,.F.);
#5277=ORIENTED_EDGE('',*,*,#3898,.F.);
#5278=ORIENTED_EDGE('',*,*,#3884,.F.);
#5279=ORIENTED_EDGE('',*,*,#3978,.F.);
#5280=ORIENTED_EDGE('',*,*,#3920,.F.);
#5281=ORIENTED_EDGE('',*,*,#3900,.F.);
#5282=ORIENTED_EDGE('',*,*,#3922,.F.);
#5283=ORIENTED_EDGE('',*,*,#3881,.F.);
#5284=ORIENTED_EDGE('',*,*,#3919,.F.);
#5285=ORIENTED_EDGE('',*,*,#3912,.F.);
#5286=ORIENTED_EDGE('',*,*,#3980,.T.);
#5287=ORIENTED_EDGE('',*,*,#3981,.T.);
#5288=ORIENTED_EDGE('',*,*,#3982,.T.);
#5289=ORIENTED_EDGE('',*,*,#3981,.F.);
#5290=ORIENTED_EDGE('',*,*,#3983,.T.);
#5291=ORIENTED_EDGE('',*,*,#3984,.T.);
#5292=ORIENTED_EDGE('',*,*,#3985,.T.);
#5293=ORIENTED_EDGE('',*,*,#3984,.F.);
#5294=ORIENTED_EDGE('',*,*,#3986,.T.);
#5295=ORIENTED_EDGE('',*,*,#3987,.T.);
#5296=ORIENTED_EDGE('',*,*,#3988,.F.);
#5297=ORIENTED_EDGE('',*,*,#3987,.F.);
#5298=ORIENTED_EDGE('',*,*,#3989,.T.);
#5299=ORIENTED_EDGE('',*,*,#3990,.T.);
#5300=ORIENTED_EDGE('',*,*,#3991,.T.);
#5301=ORIENTED_EDGE('',*,*,#3990,.F.);
#5302=ORIENTED_EDGE('',*,*,#3992,.F.);
#5303=ORIENTED_EDGE('',*,*,#3993,.T.);
#5304=ORIENTED_EDGE('',*,*,#3994,.T.);
#5305=ORIENTED_EDGE('',*,*,#3995,.T.);
#5306=ORIENTED_EDGE('',*,*,#3993,.F.);
#5307=ORIENTED_EDGE('',*,*,#3996,.T.);
#5308=ORIENTED_EDGE('',*,*,#3997,.T.);
#5309=ORIENTED_EDGE('',*,*,#3998,.F.);
#5310=ORIENTED_EDGE('',*,*,#3997,.F.);
#5311=ORIENTED_EDGE('',*,*,#3999,.T.);
#5312=ORIENTED_EDGE('',*,*,#4000,.T.);
#5313=ORIENTED_EDGE('',*,*,#4001,.F.);
#5314=ORIENTED_EDGE('',*,*,#4002,.F.);
#5315=ORIENTED_EDGE('',*,*,#4003,.T.);
#5316=ORIENTED_EDGE('',*,*,#4004,.F.);
#5317=ORIENTED_EDGE('',*,*,#4005,.T.);
#5318=ORIENTED_EDGE('',*,*,#4006,.F.);
#5319=ORIENTED_EDGE('',*,*,#4007,.T.);
#5320=ORIENTED_EDGE('',*,*,#4008,.T.);
#5321=ORIENTED_EDGE('',*,*,#4009,.T.);
#5322=ORIENTED_EDGE('',*,*,#4010,.T.);
#5323=ORIENTED_EDGE('',*,*,#4011,.T.);
#5324=ORIENTED_EDGE('',*,*,#4009,.F.);
#5325=ORIENTED_EDGE('',*,*,#4012,.T.);
#5326=ORIENTED_EDGE('',*,*,#4013,.T.);
#5327=ORIENTED_EDGE('',*,*,#4014,.F.);
#5328=ORIENTED_EDGE('',*,*,#4015,.T.);
#5329=ORIENTED_EDGE('',*,*,#4016,.F.);
#5330=ORIENTED_EDGE('',*,*,#4017,.T.);
#5331=ORIENTED_EDGE('',*,*,#4018,.F.);
#5332=ORIENTED_EDGE('',*,*,#4019,.F.);
#5333=ORIENTED_EDGE('',*,*,#3996,.F.);
#5334=ORIENTED_EDGE('',*,*,#3999,.F.);
#5335=ORIENTED_EDGE('',*,*,#3995,.F.);
#5336=ORIENTED_EDGE('',*,*,#3994,.F.);
#5337=ORIENTED_EDGE('',*,*,#4004,.T.);
#5338=ORIENTED_EDGE('',*,*,#4020,.T.);
#5339=ORIENTED_EDGE('',*,*,#4021,.F.);
#5340=ORIENTED_EDGE('',*,*,#4022,.T.);
#5341=ORIENTED_EDGE('',*,*,#4023,.F.);
#5342=ORIENTED_EDGE('',*,*,#4024,.T.);
#5343=ORIENTED_EDGE('',*,*,#4016,.T.);
#5344=ORIENTED_EDGE('',*,*,#4025,.T.);
#5345=ORIENTED_EDGE('',*,*,#4026,.F.);
#5346=ORIENTED_EDGE('',*,*,#4027,.F.);
#5347=ORIENTED_EDGE('',*,*,#4000,.F.);
#5348=ORIENTED_EDGE('',*,*,#4028,.F.);
#5349=ORIENTED_EDGE('',*,*,#4029,.T.);
#5350=ORIENTED_EDGE('',*,*,#4030,.T.);
#5351=ORIENTED_EDGE('',*,*,#4031,.T.);
#5352=ORIENTED_EDGE('',*,*,#4014,.T.);
#5353=ORIENTED_EDGE('',*,*,#4032,.T.);
#5354=ORIENTED_EDGE('',*,*,#4006,.T.);
#5355=ORIENTED_EDGE('',*,*,#4033,.T.);
#5356=ORIENTED_EDGE('',*,*,#4034,.T.);
#5357=ORIENTED_EDGE('',*,*,#4035,.F.);
#5358=ORIENTED_EDGE('',*,*,#4036,.T.);
#5359=ORIENTED_EDGE('',*,*,#4037,.T.);
#5360=ORIENTED_EDGE('',*,*,#4038,.F.);
#5361=ORIENTED_EDGE('',*,*,#4039,.T.);
#5362=ORIENTED_EDGE('',*,*,#4040,.T.);
#5363=ORIENTED_EDGE('',*,*,#4032,.F.);
#5364=ORIENTED_EDGE('',*,*,#4011,.F.);
#5365=ORIENTED_EDGE('',*,*,#4010,.F.);
#5366=ORIENTED_EDGE('',*,*,#4041,.F.);
#5367=ORIENTED_EDGE('',*,*,#4042,.F.);
#5368=ORIENTED_EDGE('',*,*,#4043,.F.);
#5369=ORIENTED_EDGE('',*,*,#4044,.F.);
#5370=ORIENTED_EDGE('',*,*,#4026,.T.);
#5371=ORIENTED_EDGE('',*,*,#4045,.T.);
#5372=ORIENTED_EDGE('',*,*,#4046,.F.);
#5373=ORIENTED_EDGE('',*,*,#4047,.F.);
#5374=ORIENTED_EDGE('',*,*,#4048,.T.);
#5375=ORIENTED_EDGE('',*,*,#4049,.T.);
#5376=ORIENTED_EDGE('',*,*,#4023,.T.);
#5377=ORIENTED_EDGE('',*,*,#4050,.T.);
#5378=ORIENTED_EDGE('',*,*,#4030,.F.);
#5379=ORIENTED_EDGE('',*,*,#4051,.F.);
#5380=ORIENTED_EDGE('',*,*,#4045,.F.);
#5381=ORIENTED_EDGE('',*,*,#4028,.T.);
#5382=ORIENTED_EDGE('',*,*,#4019,.T.);
#5383=ORIENTED_EDGE('',*,*,#3992,.T.);
#5384=ORIENTED_EDGE('',*,*,#4021,.T.);
#5385=ORIENTED_EDGE('',*,*,#4052,.T.);
#5386=ORIENTED_EDGE('',*,*,#4053,.T.);
#5387=ORIENTED_EDGE('',*,*,#4001,.T.);
#5388=ORIENTED_EDGE('',*,*,#4027,.T.);
#5389=ORIENTED_EDGE('',*,*,#4047,.T.);
#5390=ORIENTED_EDGE('',*,*,#4054,.F.);
#5391=ORIENTED_EDGE('',*,*,#4034,.F.);
#5392=ORIENTED_EDGE('',*,*,#4055,.T.);
#5393=ORIENTED_EDGE('',*,*,#3998,.T.);
#5394=ORIENTED_EDGE('',*,*,#4035,.T.);
#5395=ORIENTED_EDGE('',*,*,#4054,.T.);
#5396=ORIENTED_EDGE('',*,*,#4046,.T.);
#5397=ORIENTED_EDGE('',*,*,#4051,.T.);
#5398=ORIENTED_EDGE('',*,*,#4040,.F.);
#5399=ORIENTED_EDGE('',*,*,#4056,.T.);
#5400=ORIENTED_EDGE('',*,*,#4057,.T.);
#5401=ORIENTED_EDGE('',*,*,#4058,.F.);
#5402=ORIENTED_EDGE('',*,*,#4059,.F.);
#5403=ORIENTED_EDGE('',*,*,#4060,.T.);
#5404=ORIENTED_EDGE('',*,*,#4061,.T.);
#5405=ORIENTED_EDGE('',*,*,#4062,.F.);
#5406=ORIENTED_EDGE('',*,*,#4007,.F.);
#5407=ORIENTED_EDGE('',*,*,#4058,.T.);
#5408=ORIENTED_EDGE('',*,*,#4063,.F.);
#5409=ORIENTED_EDGE('',*,*,#4064,.T.);
#5410=ORIENTED_EDGE('',*,*,#3985,.F.);
#5411=ORIENTED_EDGE('',*,*,#4008,.F.);
#5412=ORIENTED_EDGE('',*,*,#4062,.T.);
#5413=ORIENTED_EDGE('',*,*,#4065,.T.);
#5414=ORIENTED_EDGE('',*,*,#4066,.F.);
#5415=ORIENTED_EDGE('',*,*,#4012,.F.);
#5416=ORIENTED_EDGE('',*,*,#4067,.F.);
#5417=ORIENTED_EDGE('',*,*,#4068,.T.);
#5418=ORIENTED_EDGE('',*,*,#4036,.F.);
#5419=ORIENTED_EDGE('',*,*,#4069,.T.);
#5420=ORIENTED_EDGE('',*,*,#4070,.T.);
#5421=ORIENTED_EDGE('',*,*,#4056,.F.);
#5422=ORIENTED_EDGE('',*,*,#4013,.F.);
#5423=ORIENTED_EDGE('',*,*,#4066,.T.);
#5424=ORIENTED_EDGE('',*,*,#3986,.F.);
#5425=ORIENTED_EDGE('',*,*,#4070,.F.);
#5426=ORIENTED_EDGE('',*,*,#4071,.T.);
#5427=ORIENTED_EDGE('',*,*,#4072,.T.);
#5428=ORIENTED_EDGE('',*,*,#4073,.T.);
#5429=ORIENTED_EDGE('',*,*,#4074,.T.);
#5430=ORIENTED_EDGE('',*,*,#4075,.T.);
#5431=ORIENTED_EDGE('',*,*,#4063,.T.);
#5432=ORIENTED_EDGE('',*,*,#4057,.F.);
#5433=ORIENTED_EDGE('',*,*,#4076,.F.);
#5434=ORIENTED_EDGE('',*,*,#4077,.T.);
#5435=ORIENTED_EDGE('',*,*,#4078,.F.);
#5436=ORIENTED_EDGE('',*,*,#4079,.T.);
#5437=ORIENTED_EDGE('',*,*,#4067,.T.);
#5438=ORIENTED_EDGE('',*,*,#4065,.F.);
#5439=ORIENTED_EDGE('',*,*,#4061,.F.);
#5440=ORIENTED_EDGE('',*,*,#4080,.T.);
#5441=ORIENTED_EDGE('',*,*,#4081,.F.);
#5442=ORIENTED_EDGE('',*,*,#4082,.T.);
#5443=ORIENTED_EDGE('',*,*,#4059,.T.);
#5444=ORIENTED_EDGE('',*,*,#4083,.T.);
#5445=ORIENTED_EDGE('',*,*,#4084,.T.);
#5446=ORIENTED_EDGE('',*,*,#4085,.T.);
#5447=ORIENTED_EDGE('',*,*,#4086,.F.);
#5448=ORIENTED_EDGE('',*,*,#4087,.T.);
#5449=ORIENTED_EDGE('',*,*,#4038,.T.);
#5450=ORIENTED_EDGE('',*,*,#4088,.T.);
#5451=ORIENTED_EDGE('',*,*,#4078,.T.);
#5452=ORIENTED_EDGE('',*,*,#4089,.T.);
#5453=ORIENTED_EDGE('',*,*,#4084,.F.);
#5454=ORIENTED_EDGE('',*,*,#4090,.T.);
#5455=ORIENTED_EDGE('',*,*,#4072,.F.);
#5456=ORIENTED_EDGE('',*,*,#4091,.T.);
#5457=ORIENTED_EDGE('',*,*,#3991,.F.);
#5458=ORIENTED_EDGE('',*,*,#4076,.T.);
#5459=ORIENTED_EDGE('',*,*,#4092,.T.);
#5460=ORIENTED_EDGE('',*,*,#4081,.T.);
#5461=ORIENTED_EDGE('',*,*,#4093,.T.);
#5462=ORIENTED_EDGE('',*,*,#4074,.F.);
#5463=ORIENTED_EDGE('',*,*,#4094,.T.);
#5464=ORIENTED_EDGE('',*,*,#4086,.T.);
#5465=ORIENTED_EDGE('',*,*,#4095,.T.);
#5466=ORIENTED_EDGE('',*,*,#3989,.F.);
#5467=ORIENTED_EDGE('',*,*,#3988,.T.);
#5468=ORIENTED_EDGE('',*,*,#3983,.F.);
#5469=ORIENTED_EDGE('',*,*,#4089,.F.);
#5470=ORIENTED_EDGE('',*,*,#4077,.F.);
#5471=ORIENTED_EDGE('',*,*,#4095,.F.);
#5472=ORIENTED_EDGE('',*,*,#4085,.F.);
#5473=ORIENTED_EDGE('',*,*,#4092,.F.);
#5474=ORIENTED_EDGE('',*,*,#4080,.F.);
#5475=ORIENTED_EDGE('',*,*,#4060,.F.);
#5476=ORIENTED_EDGE('',*,*,#4082,.F.);
#5477=ORIENTED_EDGE('',*,*,#4068,.F.);
#5478=ORIENTED_EDGE('',*,*,#4079,.F.);
#5479=ORIENTED_EDGE('',*,*,#4088,.F.);
#5480=ORIENTED_EDGE('',*,*,#4037,.F.);
#5481=ORIENTED_EDGE('',*,*,#4091,.F.);
#5482=ORIENTED_EDGE('',*,*,#4071,.F.);
#5483=ORIENTED_EDGE('',*,*,#4069,.F.);
#5484=ORIENTED_EDGE('',*,*,#4039,.F.);
#5485=ORIENTED_EDGE('',*,*,#4064,.F.);
#5486=ORIENTED_EDGE('',*,*,#4075,.F.);
#5487=ORIENTED_EDGE('',*,*,#4093,.F.);
#5488=ORIENTED_EDGE('',*,*,#4083,.F.);
#5489=ORIENTED_EDGE('',*,*,#4090,.F.);
#5490=ORIENTED_EDGE('',*,*,#4087,.F.);
#5491=ORIENTED_EDGE('',*,*,#4094,.F.);
#5492=ORIENTED_EDGE('',*,*,#4073,.F.);
#5493=ORIENTED_EDGE('',*,*,#4096,.T.);
#5494=ORIENTED_EDGE('',*,*,#4097,.T.);
#5495=ORIENTED_EDGE('',*,*,#4098,.T.);
#5496=ORIENTED_EDGE('',*,*,#4099,.T.);
#5497=ORIENTED_EDGE('',*,*,#4100,.T.);
#5498=ORIENTED_EDGE('',*,*,#4101,.T.);
#5499=ORIENTED_EDGE('',*,*,#4096,.F.);
#5500=ORIENTED_EDGE('',*,*,#4102,.T.);
#5501=ORIENTED_EDGE('',*,*,#4103,.F.);
#5502=ORIENTED_EDGE('',*,*,#4042,.T.);
#5503=ORIENTED_EDGE('',*,*,#3982,.F.);
#5504=ORIENTED_EDGE('',*,*,#4104,.T.);
#5505=ORIENTED_EDGE('',*,*,#4105,.T.);
#5506=ORIENTED_EDGE('',*,*,#4100,.F.);
#5507=ORIENTED_EDGE('',*,*,#4041,.T.);
#5508=ORIENTED_EDGE('',*,*,#4098,.F.);
#5509=ORIENTED_EDGE('',*,*,#4106,.T.);
#5510=ORIENTED_EDGE('',*,*,#4104,.F.);
#5511=ORIENTED_EDGE('',*,*,#4044,.T.);
#5512=ORIENTED_EDGE('',*,*,#4107,.T.);
#5513=ORIENTED_EDGE('',*,*,#4108,.T.);
#5514=ORIENTED_EDGE('',*,*,#3980,.F.);
#5515=ORIENTED_EDGE('',*,*,#4103,.T.);
#5516=ORIENTED_EDGE('',*,*,#4109,.T.);
#5517=ORIENTED_EDGE('',*,*,#4107,.F.);
#5518=ORIENTED_EDGE('',*,*,#4043,.T.);
#5519=ORIENTED_EDGE('',*,*,#4101,.F.);
#5520=ORIENTED_EDGE('',*,*,#4105,.F.);
#5521=ORIENTED_EDGE('',*,*,#4106,.F.);
#5522=ORIENTED_EDGE('',*,*,#4097,.F.);
#5523=ORIENTED_EDGE('',*,*,#4108,.F.);
#5524=ORIENTED_EDGE('',*,*,#4109,.F.);
#5525=ORIENTED_EDGE('',*,*,#4102,.F.);
#5526=ORIENTED_EDGE('',*,*,#4099,.F.);
#5527=ORIENTED_EDGE('',*,*,#4050,.F.);
#5528=ORIENTED_EDGE('',*,*,#4025,.F.);
#5529=ORIENTED_EDGE('',*,*,#4015,.F.);
#5530=ORIENTED_EDGE('',*,*,#4031,.F.);
#5531=ORIENTED_EDGE('',*,*,#4005,.F.);
#5532=ORIENTED_EDGE('',*,*,#4022,.F.);
#5533=ORIENTED_EDGE('',*,*,#4055,.F.);
#5534=ORIENTED_EDGE('',*,*,#4033,.F.);
#5535=ORIENTED_EDGE('',*,*,#4029,.F.);
#5536=ORIENTED_EDGE('',*,*,#4018,.T.);
#5537=ORIENTED_EDGE('',*,*,#4110,.T.);
#5538=ORIENTED_EDGE('',*,*,#4048,.F.);
#5539=ORIENTED_EDGE('',*,*,#4053,.F.);
#5540=ORIENTED_EDGE('',*,*,#4111,.T.);
#5541=ORIENTED_EDGE('',*,*,#4002,.T.);
#5542=ORIENTED_EDGE('',*,*,#4049,.F.);
#5543=ORIENTED_EDGE('',*,*,#4110,.F.);
#5544=ORIENTED_EDGE('',*,*,#4017,.F.);
#5545=ORIENTED_EDGE('',*,*,#4024,.F.);
#5546=ORIENTED_EDGE('',*,*,#4003,.F.);
#5547=ORIENTED_EDGE('',*,*,#4111,.F.);
#5548=ORIENTED_EDGE('',*,*,#4052,.F.);
#5549=ORIENTED_EDGE('',*,*,#4020,.F.);
#5550=ORIENTED_EDGE('',*,*,#4112,.F.);
#5551=ORIENTED_EDGE('',*,*,#4113,.T.);
#5552=ORIENTED_EDGE('',*,*,#4114,.T.);
#5553=ORIENTED_EDGE('',*,*,#4113,.F.);
#5554=ORIENTED_EDGE('',*,*,#4115,.F.);
#5555=ORIENTED_EDGE('',*,*,#4116,.T.);
#5556=ORIENTED_EDGE('',*,*,#4117,.T.);
#5557=ORIENTED_EDGE('',*,*,#4116,.F.);
#5558=ORIENTED_EDGE('',*,*,#4118,.T.);
#5559=ORIENTED_EDGE('',*,*,#4119,.T.);
#5560=ORIENTED_EDGE('',*,*,#4120,.F.);
#5561=ORIENTED_EDGE('',*,*,#4119,.F.);
#5562=ORIENTED_EDGE('',*,*,#4118,.F.);
#5563=ORIENTED_EDGE('',*,*,#4121,.F.);
#5564=ORIENTED_EDGE('',*,*,#4122,.F.);
#5565=ORIENTED_EDGE('',*,*,#4123,.F.);
#5566=ORIENTED_EDGE('',*,*,#4124,.F.);
#5567=ORIENTED_EDGE('',*,*,#4120,.T.);
#5568=ORIENTED_EDGE('',*,*,#4114,.F.);
#5569=ORIENTED_EDGE('',*,*,#4125,.T.);
#5570=ORIENTED_EDGE('',*,*,#4126,.T.);
#5571=ORIENTED_EDGE('',*,*,#4121,.T.);
#5572=ORIENTED_EDGE('',*,*,#4127,.F.);
#5573=ORIENTED_EDGE('',*,*,#4115,.T.);
#5574=ORIENTED_EDGE('',*,*,#4128,.F.);
#5575=ORIENTED_EDGE('',*,*,#4129,.T.);
#5576=ORIENTED_EDGE('',*,*,#4127,.T.);
#5577=ORIENTED_EDGE('',*,*,#4124,.T.);
#5578=ORIENTED_EDGE('',*,*,#4130,.F.);
#5579=ORIENTED_EDGE('',*,*,#4131,.T.);
#5580=ORIENTED_EDGE('',*,*,#4128,.T.);
#5581=ORIENTED_EDGE('',*,*,#4123,.T.);
#5582=ORIENTED_EDGE('',*,*,#4117,.F.);
#5583=ORIENTED_EDGE('',*,*,#4126,.F.);
#5584=ORIENTED_EDGE('',*,*,#4132,.T.);
#5585=ORIENTED_EDGE('',*,*,#4130,.T.);
#5586=ORIENTED_EDGE('',*,*,#4122,.T.);
#5587=ORIENTED_EDGE('',*,*,#4129,.F.);
#5588=ORIENTED_EDGE('',*,*,#4131,.F.);
#5589=ORIENTED_EDGE('',*,*,#4132,.F.);
#5590=ORIENTED_EDGE('',*,*,#4125,.F.);
#5591=ORIENTED_EDGE('',*,*,#4112,.T.);
#5592=ORIENTED_EDGE('',*,*,#4133,.F.);
#5593=ORIENTED_EDGE('',*,*,#4134,.T.);
#5594=ORIENTED_EDGE('',*,*,#4135,.T.);
#5595=ORIENTED_EDGE('',*,*,#4134,.F.);
#5596=ORIENTED_EDGE('',*,*,#4136,.F.);
#5597=ORIENTED_EDGE('',*,*,#4137,.F.);
#5598=ORIENTED_EDGE('',*,*,#4138,.F.);
#5599=ORIENTED_EDGE('',*,*,#4139,.F.);
#5600=ORIENTED_EDGE('',*,*,#4140,.T.);
#5601=ORIENTED_EDGE('',*,*,#4141,.T.);
#5602=ORIENTED_EDGE('',*,*,#4142,.F.);
#5603=ORIENTED_EDGE('',*,*,#4141,.F.);
#5604=ORIENTED_EDGE('',*,*,#4142,.T.);
#5605=ORIENTED_EDGE('',*,*,#4143,.F.);
#5606=ORIENTED_EDGE('',*,*,#4144,.F.);
#5607=ORIENTED_EDGE('',*,*,#4145,.F.);
#5608=ORIENTED_EDGE('',*,*,#4146,.F.);
#5609=ORIENTED_EDGE('',*,*,#4140,.F.);
#5610=ORIENTED_EDGE('',*,*,#4147,.F.);
#5611=ORIENTED_EDGE('',*,*,#4138,.T.);
#5612=ORIENTED_EDGE('',*,*,#4148,.T.);
#5613=ORIENTED_EDGE('',*,*,#4144,.T.);
#5614=ORIENTED_EDGE('',*,*,#4135,.F.);
#5615=ORIENTED_EDGE('',*,*,#4149,.F.);
#5616=ORIENTED_EDGE('',*,*,#4139,.T.);
#5617=ORIENTED_EDGE('',*,*,#4147,.T.);
#5618=ORIENTED_EDGE('',*,*,#4143,.T.);
#5619=ORIENTED_EDGE('',*,*,#4136,.T.);
#5620=ORIENTED_EDGE('',*,*,#4149,.T.);
#5621=ORIENTED_EDGE('',*,*,#4146,.T.);
#5622=ORIENTED_EDGE('',*,*,#4150,.F.);
#5623=ORIENTED_EDGE('',*,*,#4133,.T.);
#5624=ORIENTED_EDGE('',*,*,#4148,.F.);
#5625=ORIENTED_EDGE('',*,*,#4137,.T.);
#5626=ORIENTED_EDGE('',*,*,#4150,.T.);
#5627=ORIENTED_EDGE('',*,*,#4145,.T.);
#5628=ORIENTED_EDGE('',*,*,#4151,.F.);
#5629=ORIENTED_EDGE('',*,*,#4152,.T.);
#5630=ORIENTED_EDGE('',*,*,#4153,.T.);
#5631=ORIENTED_EDGE('',*,*,#4152,.F.);
#5632=ORIENTED_EDGE('',*,*,#4154,.F.);
#5633=ORIENTED_EDGE('',*,*,#4155,.T.);
#5634=ORIENTED_EDGE('',*,*,#4156,.T.);
#5635=ORIENTED_EDGE('',*,*,#4155,.F.);
#5636=ORIENTED_EDGE('',*,*,#4157,.T.);
#5637=ORIENTED_EDGE('',*,*,#4158,.T.);
#5638=ORIENTED_EDGE('',*,*,#4159,.F.);
#5639=ORIENTED_EDGE('',*,*,#4158,.F.);
#5640=ORIENTED_EDGE('',*,*,#4157,.F.);
#5641=ORIENTED_EDGE('',*,*,#4160,.F.);
#5642=ORIENTED_EDGE('',*,*,#4161,.F.);
#5643=ORIENTED_EDGE('',*,*,#4162,.F.);
#5644=ORIENTED_EDGE('',*,*,#4163,.F.);
#5645=ORIENTED_EDGE('',*,*,#4159,.T.);
#5646=ORIENTED_EDGE('',*,*,#4153,.F.);
#5647=ORIENTED_EDGE('',*,*,#4164,.T.);
#5648=ORIENTED_EDGE('',*,*,#4165,.T.);
#5649=ORIENTED_EDGE('',*,*,#4160,.T.);
#5650=ORIENTED_EDGE('',*,*,#4166,.F.);
#5651=ORIENTED_EDGE('',*,*,#4154,.T.);
#5652=ORIENTED_EDGE('',*,*,#4167,.F.);
#5653=ORIENTED_EDGE('',*,*,#4168,.T.);
#5654=ORIENTED_EDGE('',*,*,#4166,.T.);
#5655=ORIENTED_EDGE('',*,*,#4163,.T.);
#5656=ORIENTED_EDGE('',*,*,#4169,.F.);
#5657=ORIENTED_EDGE('',*,*,#4170,.T.);
#5658=ORIENTED_EDGE('',*,*,#4167,.T.);
#5659=ORIENTED_EDGE('',*,*,#4162,.T.);
#5660=ORIENTED_EDGE('',*,*,#4156,.F.);
#5661=ORIENTED_EDGE('',*,*,#4165,.F.);
#5662=ORIENTED_EDGE('',*,*,#4171,.T.);
#5663=ORIENTED_EDGE('',*,*,#4169,.T.);
#5664=ORIENTED_EDGE('',*,*,#4161,.T.);
#5665=ORIENTED_EDGE('',*,*,#4168,.F.);
#5666=ORIENTED_EDGE('',*,*,#4170,.F.);
#5667=ORIENTED_EDGE('',*,*,#4171,.F.);
#5668=ORIENTED_EDGE('',*,*,#4164,.F.);
#5669=ORIENTED_EDGE('',*,*,#4151,.T.);
#5670=ORIENTED_EDGE('',*,*,#4172,.F.);
#5671=ORIENTED_EDGE('',*,*,#4173,.T.);
#5672=ORIENTED_EDGE('',*,*,#4174,.T.);
#5673=ORIENTED_EDGE('',*,*,#4173,.F.);
#5674=ORIENTED_EDGE('',*,*,#4175,.F.);
#5675=ORIENTED_EDGE('',*,*,#4176,.F.);
#5676=ORIENTED_EDGE('',*,*,#4177,.F.);
#5677=ORIENTED_EDGE('',*,*,#4178,.F.);
#5678=ORIENTED_EDGE('',*,*,#4179,.T.);
#5679=ORIENTED_EDGE('',*,*,#4180,.T.);
#5680=ORIENTED_EDGE('',*,*,#4181,.F.);
#5681=ORIENTED_EDGE('',*,*,#4180,.F.);
#5682=ORIENTED_EDGE('',*,*,#4181,.T.);
#5683=ORIENTED_EDGE('',*,*,#4182,.F.);
#5684=ORIENTED_EDGE('',*,*,#4183,.F.);
#5685=ORIENTED_EDGE('',*,*,#4184,.F.);
#5686=ORIENTED_EDGE('',*,*,#4185,.F.);
#5687=ORIENTED_EDGE('',*,*,#4179,.F.);
#5688=ORIENTED_EDGE('',*,*,#4186,.F.);
#5689=ORIENTED_EDGE('',*,*,#4177,.T.);
#5690=ORIENTED_EDGE('',*,*,#4187,.T.);
#5691=ORIENTED_EDGE('',*,*,#4183,.T.);
#5692=ORIENTED_EDGE('',*,*,#4174,.F.);
#5693=ORIENTED_EDGE('',*,*,#4188,.F.);
#5694=ORIENTED_EDGE('',*,*,#4178,.T.);
#5695=ORIENTED_EDGE('',*,*,#4186,.T.);
#5696=ORIENTED_EDGE('',*,*,#4182,.T.);
#5697=ORIENTED_EDGE('',*,*,#4175,.T.);
#5698=ORIENTED_EDGE('',*,*,#4188,.T.);
#5699=ORIENTED_EDGE('',*,*,#4185,.T.);
#5700=ORIENTED_EDGE('',*,*,#4189,.F.);
#5701=ORIENTED_EDGE('',*,*,#4172,.T.);
#5702=ORIENTED_EDGE('',*,*,#4187,.F.);
#5703=ORIENTED_EDGE('',*,*,#4176,.T.);
#5704=ORIENTED_EDGE('',*,*,#4189,.T.);
#5705=ORIENTED_EDGE('',*,*,#4184,.T.);
#5706=ORIENTED_EDGE('',*,*,#4190,.F.);
#5707=ORIENTED_EDGE('',*,*,#4191,.T.);
#5708=ORIENTED_EDGE('',*,*,#4192,.T.);
#5709=ORIENTED_EDGE('',*,*,#4191,.F.);
#5710=ORIENTED_EDGE('',*,*,#4193,.F.);
#5711=ORIENTED_EDGE('',*,*,#4194,.T.);
#5712=ORIENTED_EDGE('',*,*,#4195,.T.);
#5713=ORIENTED_EDGE('',*,*,#4194,.F.);
#5714=ORIENTED_EDGE('',*,*,#4196,.T.);
#5715=ORIENTED_EDGE('',*,*,#4197,.T.);
#5716=ORIENTED_EDGE('',*,*,#4198,.F.);
#5717=ORIENTED_EDGE('',*,*,#4197,.F.);
#5718=ORIENTED_EDGE('',*,*,#4196,.F.);
#5719=ORIENTED_EDGE('',*,*,#4199,.F.);
#5720=ORIENTED_EDGE('',*,*,#4200,.F.);
#5721=ORIENTED_EDGE('',*,*,#4201,.F.);
#5722=ORIENTED_EDGE('',*,*,#4202,.F.);
#5723=ORIENTED_EDGE('',*,*,#4198,.T.);
#5724=ORIENTED_EDGE('',*,*,#4192,.F.);
#5725=ORIENTED_EDGE('',*,*,#4203,.T.);
#5726=ORIENTED_EDGE('',*,*,#4204,.T.);
#5727=ORIENTED_EDGE('',*,*,#4199,.T.);
#5728=ORIENTED_EDGE('',*,*,#4205,.F.);
#5729=ORIENTED_EDGE('',*,*,#4193,.T.);
#5730=ORIENTED_EDGE('',*,*,#4206,.F.);
#5731=ORIENTED_EDGE('',*,*,#4207,.T.);
#5732=ORIENTED_EDGE('',*,*,#4205,.T.);
#5733=ORIENTED_EDGE('',*,*,#4202,.T.);
#5734=ORIENTED_EDGE('',*,*,#4208,.F.);
#5735=ORIENTED_EDGE('',*,*,#4209,.T.);
#5736=ORIENTED_EDGE('',*,*,#4206,.T.);
#5737=ORIENTED_EDGE('',*,*,#4201,.T.);
#5738=ORIENTED_EDGE('',*,*,#4195,.F.);
#5739=ORIENTED_EDGE('',*,*,#4204,.F.);
#5740=ORIENTED_EDGE('',*,*,#4210,.T.);
#5741=ORIENTED_EDGE('',*,*,#4208,.T.);
#5742=ORIENTED_EDGE('',*,*,#4200,.T.);
#5743=ORIENTED_EDGE('',*,*,#4207,.F.);
#5744=ORIENTED_EDGE('',*,*,#4209,.F.);
#5745=ORIENTED_EDGE('',*,*,#4210,.F.);
#5746=ORIENTED_EDGE('',*,*,#4203,.F.);
#5747=ORIENTED_EDGE('',*,*,#4190,.T.);
#5748=ORIENTED_EDGE('',*,*,#4211,.F.);
#5749=ORIENTED_EDGE('',*,*,#4212,.T.);
#5750=ORIENTED_EDGE('',*,*,#4213,.T.);
#5751=ORIENTED_EDGE('',*,*,#4212,.F.);
#5752=ORIENTED_EDGE('',*,*,#4214,.F.);
#5753=ORIENTED_EDGE('',*,*,#4215,.F.);
#5754=ORIENTED_EDGE('',*,*,#4216,.F.);
#5755=ORIENTED_EDGE('',*,*,#4217,.F.);
#5756=ORIENTED_EDGE('',*,*,#4218,.T.);
#5757=ORIENTED_EDGE('',*,*,#4219,.T.);
#5758=ORIENTED_EDGE('',*,*,#4220,.F.);
#5759=ORIENTED_EDGE('',*,*,#4219,.F.);
#5760=ORIENTED_EDGE('',*,*,#4220,.T.);
#5761=ORIENTED_EDGE('',*,*,#4221,.F.);
#5762=ORIENTED_EDGE('',*,*,#4222,.F.);
#5763=ORIENTED_EDGE('',*,*,#4223,.F.);
#5764=ORIENTED_EDGE('',*,*,#4224,.F.);
#5765=ORIENTED_EDGE('',*,*,#4218,.F.);
#5766=ORIENTED_EDGE('',*,*,#4225,.F.);
#5767=ORIENTED_EDGE('',*,*,#4216,.T.);
#5768=ORIENTED_EDGE('',*,*,#4226,.T.);
#5769=ORIENTED_EDGE('',*,*,#4222,.T.);
#5770=ORIENTED_EDGE('',*,*,#4213,.F.);
#5771=ORIENTED_EDGE('',*,*,#4227,.F.);
#5772=ORIENTED_EDGE('',*,*,#4217,.T.);
#5773=ORIENTED_EDGE('',*,*,#4225,.T.);
#5774=ORIENTED_EDGE('',*,*,#4221,.T.);
#5775=ORIENTED_EDGE('',*,*,#4214,.T.);
#5776=ORIENTED_EDGE('',*,*,#4227,.T.);
#5777=ORIENTED_EDGE('',*,*,#4224,.T.);
#5778=ORIENTED_EDGE('',*,*,#4228,.F.);
#5779=ORIENTED_EDGE('',*,*,#4211,.T.);
#5780=ORIENTED_EDGE('',*,*,#4226,.F.);
#5781=ORIENTED_EDGE('',*,*,#4215,.T.);
#5782=ORIENTED_EDGE('',*,*,#4228,.T.);
#5783=ORIENTED_EDGE('',*,*,#4223,.T.);
#5784=ORIENTED_EDGE('',*,*,#4229,.T.);
#5785=ORIENTED_EDGE('',*,*,#4230,.T.);
#5786=ORIENTED_EDGE('',*,*,#4231,.F.);
#5787=ORIENTED_EDGE('',*,*,#4230,.F.);
#5788=ORIENTED_EDGE('',*,*,#4232,.T.);
#5789=ORIENTED_EDGE('',*,*,#4233,.T.);
#5790=ORIENTED_EDGE('',*,*,#4234,.T.);
#5791=ORIENTED_EDGE('',*,*,#4233,.F.);
#5792=ORIENTED_EDGE('',*,*,#4235,.T.);
#5793=ORIENTED_EDGE('',*,*,#4236,.T.);
#5794=ORIENTED_EDGE('',*,*,#4237,.T.);
#5795=ORIENTED_EDGE('',*,*,#4236,.F.);
#5796=ORIENTED_EDGE('',*,*,#4238,.F.);
#5797=ORIENTED_EDGE('',*,*,#4239,.T.);
#5798=ORIENTED_EDGE('',*,*,#4240,.T.);
#5799=ORIENTED_EDGE('',*,*,#4241,.T.);
#5800=ORIENTED_EDGE('',*,*,#4242,.T.);
#5801=ORIENTED_EDGE('',*,*,#4243,.F.);
#5802=ORIENTED_EDGE('',*,*,#4244,.F.);
#5803=ORIENTED_EDGE('',*,*,#4240,.F.);
#5804=ORIENTED_EDGE('',*,*,#4245,.T.);
#5805=ORIENTED_EDGE('',*,*,#4246,.T.);
#5806=ORIENTED_EDGE('',*,*,#4229,.F.);
#5807=ORIENTED_EDGE('',*,*,#4247,.T.);
#5808=ORIENTED_EDGE('',*,*,#4248,.F.);
#5809=ORIENTED_EDGE('',*,*,#4249,.F.);
#5810=ORIENTED_EDGE('',*,*,#4243,.T.);
#5811=ORIENTED_EDGE('',*,*,#4250,.T.);
#5812=ORIENTED_EDGE('',*,*,#4251,.F.);
#5813=ORIENTED_EDGE('',*,*,#4252,.F.);
#5814=ORIENTED_EDGE('',*,*,#4253,.F.);
#5815=ORIENTED_EDGE('',*,*,#4254,.T.);
#5816=ORIENTED_EDGE('',*,*,#4248,.T.);
#5817=ORIENTED_EDGE('',*,*,#4234,.F.);
#5818=ORIENTED_EDGE('',*,*,#4255,.T.);
#5819=ORIENTED_EDGE('',*,*,#4246,.F.);
#5820=ORIENTED_EDGE('',*,*,#4256,.F.);
#5821=ORIENTED_EDGE('',*,*,#4251,.T.);
#5822=ORIENTED_EDGE('',*,*,#4242,.F.);
#5823=ORIENTED_EDGE('',*,*,#4255,.F.);
#5824=ORIENTED_EDGE('',*,*,#4250,.F.);
#5825=ORIENTED_EDGE('',*,*,#4247,.F.);
#5826=ORIENTED_EDGE('',*,*,#4239,.F.);
#5827=ORIENTED_EDGE('',*,*,#4257,.F.);
#5828=ORIENTED_EDGE('',*,*,#4258,.F.);
#5829=ORIENTED_EDGE('',*,*,#4259,.F.);
#5830=ORIENTED_EDGE('',*,*,#4260,.F.);
#5831=ORIENTED_EDGE('',*,*,#4252,.T.);
#5832=ORIENTED_EDGE('',*,*,#4256,.T.);
#5833=ORIENTED_EDGE('',*,*,#4245,.F.);
#5834=ORIENTED_EDGE('',*,*,#4261,.F.);
#5835=ORIENTED_EDGE('',*,*,#4262,.F.);
#5836=ORIENTED_EDGE('',*,*,#4241,.F.);
#5837=ORIENTED_EDGE('',*,*,#4244,.T.);
#5838=ORIENTED_EDGE('',*,*,#4249,.T.);
#5839=ORIENTED_EDGE('',*,*,#4254,.F.);
#5840=ORIENTED_EDGE('',*,*,#4263,.F.);
#5841=ORIENTED_EDGE('',*,*,#4264,.F.);
#5842=ORIENTED_EDGE('',*,*,#4265,.F.);
#5843=ORIENTED_EDGE('',*,*,#4263,.T.);
#5844=ORIENTED_EDGE('',*,*,#4253,.T.);
#5845=ORIENTED_EDGE('',*,*,#4260,.T.);
#5846=ORIENTED_EDGE('',*,*,#4238,.T.);
#5847=ORIENTED_EDGE('',*,*,#4262,.T.);
#5848=ORIENTED_EDGE('',*,*,#4266,.F.);
#5849=ORIENTED_EDGE('',*,*,#4257,.T.);
#5850=ORIENTED_EDGE('',*,*,#4237,.F.);
#5851=ORIENTED_EDGE('',*,*,#4265,.T.);
#5852=ORIENTED_EDGE('',*,*,#4259,.T.);
#5853=ORIENTED_EDGE('',*,*,#4267,.T.);
#5854=ORIENTED_EDGE('',*,*,#4264,.T.);
#5855=ORIENTED_EDGE('',*,*,#4235,.F.);
#5856=ORIENTED_EDGE('',*,*,#4258,.T.);
#5857=ORIENTED_EDGE('',*,*,#4266,.T.);
#5858=ORIENTED_EDGE('',*,*,#4261,.T.);
#5859=ORIENTED_EDGE('',*,*,#4267,.F.);
#5860=ORIENTED_EDGE('',*,*,#4232,.F.);
#5861=ORIENTED_EDGE('',*,*,#4231,.T.);
#5862=ORIENTED_EDGE('',*,*,#4268,.T.);
#5863=ORIENTED_EDGE('',*,*,#4269,.T.);
#5864=ORIENTED_EDGE('',*,*,#4270,.T.);
#5865=ORIENTED_EDGE('',*,*,#4271,.T.);
#5866=ORIENTED_EDGE('',*,*,#4269,.F.);
#5867=ORIENTED_EDGE('',*,*,#4272,.T.);
#5868=ORIENTED_EDGE('',*,*,#4273,.T.);
#5869=ORIENTED_EDGE('',*,*,#4274,.T.);
#5870=ORIENTED_EDGE('',*,*,#4273,.F.);
#5871=ORIENTED_EDGE('',*,*,#4275,.T.);
#5872=ORIENTED_EDGE('',*,*,#4276,.F.);
#5873=ORIENTED_EDGE('',*,*,#4277,.T.);
#5874=ORIENTED_EDGE('',*,*,#4277,.F.);
#5875=ORIENTED_EDGE('',*,*,#4278,.F.);
#5876=ORIENTED_EDGE('',*,*,#4279,.T.);
#5877=ORIENTED_EDGE('',*,*,#4276,.T.);
#5878=ORIENTED_EDGE('',*,*,#4279,.F.);
#5879=ORIENTED_EDGE('',*,*,#4271,.F.);
#5880=ORIENTED_EDGE('',*,*,#4270,.F.);
#5881=ORIENTED_EDGE('',*,*,#4272,.F.);
#5882=ORIENTED_EDGE('',*,*,#4275,.F.);
#5883=ORIENTED_EDGE('',*,*,#4278,.T.);
#5884=ORIENTED_EDGE('',*,*,#4280,.T.);
#5885=ORIENTED_EDGE('',*,*,#4281,.T.);
#5886=ORIENTED_EDGE('',*,*,#4282,.T.);
#5887=ORIENTED_EDGE('',*,*,#4283,.T.);
#5888=ORIENTED_EDGE('',*,*,#4284,.T.);
#5889=ORIENTED_EDGE('',*,*,#4285,.T.);
#5890=ORIENTED_EDGE('',*,*,#4286,.T.);
#5891=ORIENTED_EDGE('',*,*,#4287,.T.);
#5892=ORIENTED_EDGE('',*,*,#4283,.F.);
#5893=ORIENTED_EDGE('',*,*,#4288,.F.);
#5894=ORIENTED_EDGE('',*,*,#4285,.F.);
#5895=ORIENTED_EDGE('',*,*,#4289,.T.);
#5896=ORIENTED_EDGE('',*,*,#4282,.F.);
#5897=ORIENTED_EDGE('',*,*,#4290,.F.);
#5898=ORIENTED_EDGE('',*,*,#4286,.F.);
#5899=ORIENTED_EDGE('',*,*,#4288,.T.);
#5900=ORIENTED_EDGE('',*,*,#4268,.F.);
#5901=ORIENTED_EDGE('',*,*,#4281,.F.);
#5902=ORIENTED_EDGE('',*,*,#4291,.F.);
#5903=ORIENTED_EDGE('',*,*,#4287,.F.);
#5904=ORIENTED_EDGE('',*,*,#4290,.T.);
#5905=ORIENTED_EDGE('',*,*,#4280,.F.);
#5906=ORIENTED_EDGE('',*,*,#4289,.F.);
#5907=ORIENTED_EDGE('',*,*,#4284,.F.);
#5908=ORIENTED_EDGE('',*,*,#4291,.T.);
#5909=ORIENTED_EDGE('',*,*,#4274,.F.);
#5910=ORIENTED_EDGE('',*,*,#4292,.F.);
#5911=ORIENTED_EDGE('',*,*,#4293,.T.);
#5912=ORIENTED_EDGE('',*,*,#4294,.T.);
#5913=ORIENTED_EDGE('',*,*,#4293,.F.);
#5914=ORIENTED_EDGE('',*,*,#4295,.F.);
#5915=ORIENTED_EDGE('',*,*,#4296,.T.);
#5916=ORIENTED_EDGE('',*,*,#4297,.T.);
#5917=ORIENTED_EDGE('',*,*,#4296,.F.);
#5918=ORIENTED_EDGE('',*,*,#4298,.F.);
#5919=ORIENTED_EDGE('',*,*,#4299,.T.);
#5920=ORIENTED_EDGE('',*,*,#4300,.T.);
#5921=ORIENTED_EDGE('',*,*,#4299,.F.);
#5922=ORIENTED_EDGE('',*,*,#4301,.T.);
#5923=ORIENTED_EDGE('',*,*,#4302,.T.);
#5924=ORIENTED_EDGE('',*,*,#4303,.F.);
#5925=ORIENTED_EDGE('',*,*,#4302,.F.);
#5926=ORIENTED_EDGE('',*,*,#4300,.F.);
#5927=ORIENTED_EDGE('',*,*,#4304,.T.);
#5928=ORIENTED_EDGE('',*,*,#4305,.F.);
#5929=ORIENTED_EDGE('',*,*,#4306,.F.);
#5930=ORIENTED_EDGE('',*,*,#4307,.F.);
#5931=ORIENTED_EDGE('',*,*,#4308,.T.);
#5932=ORIENTED_EDGE('',*,*,#4301,.F.);
#5933=ORIENTED_EDGE('',*,*,#4308,.F.);
#5934=ORIENTED_EDGE('',*,*,#4309,.F.);
#5935=ORIENTED_EDGE('',*,*,#4310,.F.);
#5936=ORIENTED_EDGE('',*,*,#4311,.F.);
#5937=ORIENTED_EDGE('',*,*,#4304,.F.);
#5938=ORIENTED_EDGE('',*,*,#4312,.F.);
#5939=ORIENTED_EDGE('',*,*,#4313,.F.);
#5940=ORIENTED_EDGE('',*,*,#4314,.F.);
#5941=ORIENTED_EDGE('',*,*,#4315,.F.);
#5942=ORIENTED_EDGE('',*,*,#4316,.T.);
#5943=ORIENTED_EDGE('',*,*,#4317,.T.);
#5944=ORIENTED_EDGE('',*,*,#4318,.F.);
#5945=ORIENTED_EDGE('',*,*,#4319,.F.);
#5946=ORIENTED_EDGE('',*,*,#4320,.F.);
#5947=ORIENTED_EDGE('',*,*,#4321,.T.);
#5948=ORIENTED_EDGE('',*,*,#4322,.T.);
#5949=ORIENTED_EDGE('',*,*,#4323,.T.);
#5950=ORIENTED_EDGE('',*,*,#4316,.F.);
#5951=ORIENTED_EDGE('',*,*,#4324,.F.);
#5952=ORIENTED_EDGE('',*,*,#4325,.T.);
#5953=ORIENTED_EDGE('',*,*,#4326,.T.);
#5954=ORIENTED_EDGE('',*,*,#4324,.T.);
#5955=ORIENTED_EDGE('',*,*,#4319,.T.);
#5956=ORIENTED_EDGE('',*,*,#4327,.F.);
#5957=ORIENTED_EDGE('',*,*,#4328,.F.);
#5958=ORIENTED_EDGE('',*,*,#4295,.T.);
#5959=ORIENTED_EDGE('',*,*,#4327,.T.);
#5960=ORIENTED_EDGE('',*,*,#4318,.T.);
#5961=ORIENTED_EDGE('',*,*,#4329,.F.);
#5962=ORIENTED_EDGE('',*,*,#4330,.F.);
#5963=ORIENTED_EDGE('',*,*,#4317,.F.);
#5964=ORIENTED_EDGE('',*,*,#4326,.F.);
#5965=ORIENTED_EDGE('',*,*,#4331,.T.);
#5966=ORIENTED_EDGE('',*,*,#4329,.T.);
#5967=ORIENTED_EDGE('',*,*,#4297,.F.);
#5968=ORIENTED_EDGE('',*,*,#4325,.F.);
#5969=ORIENTED_EDGE('',*,*,#4328,.T.);
#5970=ORIENTED_EDGE('',*,*,#4330,.T.);
#5971=ORIENTED_EDGE('',*,*,#4331,.F.);
#5972=ORIENTED_EDGE('',*,*,#4305,.T.);
#5973=ORIENTED_EDGE('',*,*,#4311,.T.);
#5974=ORIENTED_EDGE('',*,*,#4332,.T.);
#5975=ORIENTED_EDGE('',*,*,#4333,.F.);
#5976=ORIENTED_EDGE('',*,*,#4298,.T.);
#5977=ORIENTED_EDGE('',*,*,#4310,.T.);
#5978=ORIENTED_EDGE('',*,*,#4334,.T.);
#5979=ORIENTED_EDGE('',*,*,#4335,.F.);
#5980=ORIENTED_EDGE('',*,*,#4332,.F.);
#5981=ORIENTED_EDGE('',*,*,#4309,.T.);
#5982=ORIENTED_EDGE('',*,*,#4307,.T.);
#5983=ORIENTED_EDGE('',*,*,#4336,.F.);
#5984=ORIENTED_EDGE('',*,*,#4334,.F.);
#5985=ORIENTED_EDGE('',*,*,#4303,.T.);
#5986=ORIENTED_EDGE('',*,*,#4306,.T.);
#5987=ORIENTED_EDGE('',*,*,#4333,.T.);
#5988=ORIENTED_EDGE('',*,*,#4335,.T.);
#5989=ORIENTED_EDGE('',*,*,#4336,.T.);
#5990=ORIENTED_EDGE('',*,*,#4337,.T.);
#5991=ORIENTED_EDGE('',*,*,#4338,.T.);
#5992=ORIENTED_EDGE('',*,*,#4323,.F.);
#5993=ORIENTED_EDGE('',*,*,#4339,.T.);
#5994=ORIENTED_EDGE('',*,*,#4314,.T.);
#5995=ORIENTED_EDGE('',*,*,#4340,.F.);
#5996=ORIENTED_EDGE('',*,*,#4341,.F.);
#5997=ORIENTED_EDGE('',*,*,#4342,.T.);
#5998=ORIENTED_EDGE('',*,*,#4340,.T.);
#5999=ORIENTED_EDGE('',*,*,#4313,.T.);
#6000=ORIENTED_EDGE('',*,*,#4343,.F.);
#6001=ORIENTED_EDGE('',*,*,#4344,.F.);
#6002=ORIENTED_EDGE('',*,*,#4321,.F.);
#6003=ORIENTED_EDGE('',*,*,#4345,.F.);
#6004=ORIENTED_EDGE('',*,*,#4346,.F.);
#6005=ORIENTED_EDGE('',*,*,#4347,.F.);
#6006=ORIENTED_EDGE('',*,*,#4348,.F.);
#6007=ORIENTED_EDGE('',*,*,#4343,.T.);
#6008=ORIENTED_EDGE('',*,*,#4312,.T.);
#6009=ORIENTED_EDGE('',*,*,#4349,.F.);
#6010=ORIENTED_EDGE('',*,*,#4349,.T.);
#6011=ORIENTED_EDGE('',*,*,#4315,.T.);
#6012=ORIENTED_EDGE('',*,*,#4339,.F.);
#6013=ORIENTED_EDGE('',*,*,#4322,.F.);
#6014=ORIENTED_EDGE('',*,*,#4350,.F.);
#6015=ORIENTED_EDGE('',*,*,#4341,.T.);
#6016=ORIENTED_EDGE('',*,*,#4344,.T.);
#6017=ORIENTED_EDGE('',*,*,#4348,.T.);
#6018=ORIENTED_EDGE('',*,*,#4351,.T.);
#6019=ORIENTED_EDGE('',*,*,#4346,.T.);
#6020=ORIENTED_EDGE('',*,*,#4352,.F.);
#6021=ORIENTED_EDGE('',*,*,#4337,.F.);
#6022=ORIENTED_EDGE('',*,*,#4352,.T.);
#6023=ORIENTED_EDGE('',*,*,#4345,.T.);
#6024=ORIENTED_EDGE('',*,*,#4320,.T.);
#6025=ORIENTED_EDGE('',*,*,#4338,.F.);
#6026=ORIENTED_EDGE('',*,*,#4292,.T.);
#6027=ORIENTED_EDGE('',*,*,#4350,.T.);
#6028=ORIENTED_EDGE('',*,*,#4347,.T.);
#6029=ORIENTED_EDGE('',*,*,#4351,.F.);
#6030=ORIENTED_EDGE('',*,*,#4342,.F.);
#6031=ORIENTED_EDGE('',*,*,#4294,.F.);
#6032=ORIENTED_EDGE('',*,*,#4353,.F.);
#6033=ORIENTED_EDGE('',*,*,#4354,.T.);
#6034=ORIENTED_EDGE('',*,*,#4355,.T.);
#6035=ORIENTED_EDGE('',*,*,#4354,.F.);
#6036=ORIENTED_EDGE('',*,*,#4356,.F.);
#6037=ORIENTED_EDGE('',*,*,#4357,.T.);
#6038=ORIENTED_EDGE('',*,*,#4358,.T.);
#6039=ORIENTED_EDGE('',*,*,#4359,.T.);
#6040=ORIENTED_EDGE('',*,*,#4357,.F.);
#6041=ORIENTED_EDGE('',*,*,#4360,.T.);
#6042=ORIENTED_EDGE('',*,*,#4361,.T.);
#6043=ORIENTED_EDGE('',*,*,#4362,.F.);
#6044=ORIENTED_EDGE('',*,*,#4361,.F.);
#6045=ORIENTED_EDGE('',*,*,#4363,.T.);
#6046=ORIENTED_EDGE('',*,*,#4364,.T.);
#6047=ORIENTED_EDGE('',*,*,#4365,.T.);
#6048=ORIENTED_EDGE('',*,*,#4366,.T.);
#6049=ORIENTED_EDGE('',*,*,#4367,.T.);
#6050=ORIENTED_EDGE('',*,*,#4368,.F.);
#6051=ORIENTED_EDGE('',*,*,#4369,.T.);
#6052=ORIENTED_EDGE('',*,*,#4364,.F.);
#6053=ORIENTED_EDGE('',*,*,#4370,.T.);
#6054=ORIENTED_EDGE('',*,*,#4371,.F.);
#6055=ORIENTED_EDGE('',*,*,#4372,.T.);
#6056=ORIENTED_EDGE('',*,*,#4373,.F.);
#6057=ORIENTED_EDGE('',*,*,#4374,.F.);
#6058=ORIENTED_EDGE('',*,*,#4366,.F.);
#6059=ORIENTED_EDGE('',*,*,#4375,.T.);
#6060=ORIENTED_EDGE('',*,*,#4376,.F.);
#6061=ORIENTED_EDGE('',*,*,#4377,.F.);
#6062=ORIENTED_EDGE('',*,*,#4378,.F.);
#6063=ORIENTED_EDGE('',*,*,#4379,.T.);
#6064=ORIENTED_EDGE('',*,*,#4379,.F.);
#6065=ORIENTED_EDGE('',*,*,#4380,.F.);
#6066=ORIENTED_EDGE('',*,*,#4372,.F.);
#6067=ORIENTED_EDGE('',*,*,#4381,.F.);
#6068=ORIENTED_EDGE('',*,*,#4382,.F.);
#6069=ORIENTED_EDGE('',*,*,#4383,.F.);
#6070=ORIENTED_EDGE('',*,*,#4384,.F.);
#6071=ORIENTED_EDGE('',*,*,#4385,.F.);
#6072=ORIENTED_EDGE('',*,*,#4386,.F.);
#6073=ORIENTED_EDGE('',*,*,#4387,.F.);
#6074=ORIENTED_EDGE('',*,*,#4370,.F.);
#6075=ORIENTED_EDGE('',*,*,#4367,.F.);
#6076=ORIENTED_EDGE('',*,*,#4359,.F.);
#6077=ORIENTED_EDGE('',*,*,#4358,.F.);
#6078=ORIENTED_EDGE('',*,*,#4360,.F.);
#6079=ORIENTED_EDGE('',*,*,#4363,.F.);
#6080=ORIENTED_EDGE('',*,*,#4381,.T.);
#6081=ORIENTED_EDGE('',*,*,#4371,.T.);
#6082=ORIENTED_EDGE('',*,*,#4387,.T.);
#6083=ORIENTED_EDGE('',*,*,#4388,.T.);
#6084=ORIENTED_EDGE('',*,*,#4389,.F.);
#6085=ORIENTED_EDGE('',*,*,#4373,.T.);
#6086=ORIENTED_EDGE('',*,*,#4380,.T.);
#6087=ORIENTED_EDGE('',*,*,#4378,.T.);
#6088=ORIENTED_EDGE('',*,*,#4390,.F.);
#6089=ORIENTED_EDGE('',*,*,#4391,.T.);
#6090=ORIENTED_EDGE('',*,*,#4384,.T.);
#6091=ORIENTED_EDGE('',*,*,#4392,.T.);
#6092=ORIENTED_EDGE('',*,*,#4385,.T.);
#6093=ORIENTED_EDGE('',*,*,#4391,.F.);
#6094=ORIENTED_EDGE('',*,*,#4393,.F.);
#6095=ORIENTED_EDGE('',*,*,#4394,.F.);
#6096=ORIENTED_EDGE('',*,*,#4356,.T.);
#6097=ORIENTED_EDGE('',*,*,#4383,.T.);
#6098=ORIENTED_EDGE('',*,*,#4395,.T.);
#6099=ORIENTED_EDGE('',*,*,#4396,.F.);
#6100=ORIENTED_EDGE('',*,*,#4392,.F.);
#6101=ORIENTED_EDGE('',*,*,#4362,.T.);
#6102=ORIENTED_EDGE('',*,*,#4382,.T.);
#6103=ORIENTED_EDGE('',*,*,#4388,.F.);
#6104=ORIENTED_EDGE('',*,*,#4386,.T.);
#6105=ORIENTED_EDGE('',*,*,#4394,.T.);
#6106=ORIENTED_EDGE('',*,*,#4397,.F.);
#6107=ORIENTED_EDGE('',*,*,#4395,.F.);
#6108=ORIENTED_EDGE('',*,*,#4390,.T.);
#6109=ORIENTED_EDGE('',*,*,#4396,.T.);
#6110=ORIENTED_EDGE('',*,*,#4397,.T.);
#6111=ORIENTED_EDGE('',*,*,#4393,.T.);
#6112=ORIENTED_EDGE('',*,*,#4398,.T.);
#6113=ORIENTED_EDGE('',*,*,#4368,.T.);
#6114=ORIENTED_EDGE('',*,*,#4399,.F.);
#6115=ORIENTED_EDGE('',*,*,#4400,.F.);
#6116=ORIENTED_EDGE('',*,*,#4400,.T.);
#6117=ORIENTED_EDGE('',*,*,#4401,.F.);
#6118=ORIENTED_EDGE('',*,*,#4402,.F.);
#6119=ORIENTED_EDGE('',*,*,#4403,.T.);
#6120=ORIENTED_EDGE('',*,*,#4404,.F.);
#6121=ORIENTED_EDGE('',*,*,#4376,.T.);
#6122=ORIENTED_EDGE('',*,*,#4405,.T.);
#6123=ORIENTED_EDGE('',*,*,#4402,.T.);
#6124=ORIENTED_EDGE('',*,*,#4369,.F.);
#6125=ORIENTED_EDGE('',*,*,#4398,.F.);
#6126=ORIENTED_EDGE('',*,*,#4403,.F.);
#6127=ORIENTED_EDGE('',*,*,#4405,.F.);
#6128=ORIENTED_EDGE('',*,*,#4375,.F.);
#6129=ORIENTED_EDGE('',*,*,#4365,.F.);
#6130=ORIENTED_EDGE('',*,*,#4353,.T.);
#6131=ORIENTED_EDGE('',*,*,#4399,.T.);
#6132=ORIENTED_EDGE('',*,*,#4374,.T.);
#6133=ORIENTED_EDGE('',*,*,#4389,.T.);
#6134=ORIENTED_EDGE('',*,*,#4377,.T.);
#6135=ORIENTED_EDGE('',*,*,#4404,.T.);
#6136=ORIENTED_EDGE('',*,*,#4401,.T.);
#6137=ORIENTED_EDGE('',*,*,#4355,.F.);
#6138=ORIENTED_EDGE('',*,*,#4406,.F.);
#6139=ORIENTED_EDGE('',*,*,#4407,.T.);
#6140=ORIENTED_EDGE('',*,*,#4408,.T.);
#6141=ORIENTED_EDGE('',*,*,#4409,.T.);
#6142=ORIENTED_EDGE('',*,*,#4407,.F.);
#6143=ORIENTED_EDGE('',*,*,#4410,.T.);
#6144=ORIENTED_EDGE('',*,*,#4411,.T.);
#6145=ORIENTED_EDGE('',*,*,#4412,.F.);
#6146=ORIENTED_EDGE('',*,*,#4411,.F.);
#6147=ORIENTED_EDGE('',*,*,#4413,.T.);
#6148=ORIENTED_EDGE('',*,*,#4414,.T.);
#6149=ORIENTED_EDGE('',*,*,#4415,.F.);
#6150=ORIENTED_EDGE('',*,*,#4416,.F.);
#6151=ORIENTED_EDGE('',*,*,#4417,.F.);
#6152=ORIENTED_EDGE('',*,*,#4418,.T.);
#6153=ORIENTED_EDGE('',*,*,#4419,.F.);
#6154=ORIENTED_EDGE('',*,*,#4420,.F.);
#6155=ORIENTED_EDGE('',*,*,#4421,.F.);
#6156=ORIENTED_EDGE('',*,*,#4422,.F.);
#6157=ORIENTED_EDGE('',*,*,#4423,.F.);
#6158=ORIENTED_EDGE('',*,*,#4424,.T.);
#6159=ORIENTED_EDGE('',*,*,#4425,.T.);
#6160=ORIENTED_EDGE('',*,*,#4426,.T.);
#6161=ORIENTED_EDGE('',*,*,#4425,.F.);
#6162=ORIENTED_EDGE('',*,*,#4427,.T.);
#6163=ORIENTED_EDGE('',*,*,#4428,.T.);
#6164=ORIENTED_EDGE('',*,*,#4429,.F.);
#6165=ORIENTED_EDGE('',*,*,#4428,.F.);
#6166=ORIENTED_EDGE('',*,*,#4430,.T.);
#6167=ORIENTED_EDGE('',*,*,#4431,.T.);
#6168=ORIENTED_EDGE('',*,*,#4432,.T.);
#6169=ORIENTED_EDGE('',*,*,#4431,.F.);
#6170=ORIENTED_EDGE('',*,*,#4433,.F.);
#6171=ORIENTED_EDGE('',*,*,#4434,.T.);
#6172=ORIENTED_EDGE('',*,*,#4435,.T.);
#6173=ORIENTED_EDGE('',*,*,#4436,.F.);
#6174=ORIENTED_EDGE('',*,*,#4437,.F.);
#6175=ORIENTED_EDGE('',*,*,#4438,.F.);
#6176=ORIENTED_EDGE('',*,*,#4439,.T.);
#6177=ORIENTED_EDGE('',*,*,#4440,.T.);
#6178=ORIENTED_EDGE('',*,*,#4441,.F.);
#6179=ORIENTED_EDGE('',*,*,#4442,.T.);
#6180=ORIENTED_EDGE('',*,*,#4443,.T.);
#6181=ORIENTED_EDGE('',*,*,#4444,.T.);
#6182=ORIENTED_EDGE('',*,*,#4410,.F.);
#6183=ORIENTED_EDGE('',*,*,#4413,.F.);
#6184=ORIENTED_EDGE('',*,*,#4409,.F.);
#6185=ORIENTED_EDGE('',*,*,#4408,.F.);
#6186=ORIENTED_EDGE('',*,*,#4445,.T.);
#6187=ORIENTED_EDGE('',*,*,#4415,.T.);
#6188=ORIENTED_EDGE('',*,*,#4446,.T.);
#6189=ORIENTED_EDGE('',*,*,#4447,.F.);
#6190=ORIENTED_EDGE('',*,*,#4416,.T.);
#6191=ORIENTED_EDGE('',*,*,#4445,.F.);
#6192=ORIENTED_EDGE('',*,*,#4448,.T.);
#6193=ORIENTED_EDGE('',*,*,#4449,.T.);
#6194=ORIENTED_EDGE('',*,*,#4422,.T.);
#6195=ORIENTED_EDGE('',*,*,#4450,.F.);
#6196=ORIENTED_EDGE('',*,*,#4451,.T.);
#6197=ORIENTED_EDGE('',*,*,#4452,.T.);
#6198=ORIENTED_EDGE('',*,*,#4453,.T.);
#6199=ORIENTED_EDGE('',*,*,#4454,.F.);
#6200=ORIENTED_EDGE('',*,*,#4455,.T.);
#6201=ORIENTED_EDGE('',*,*,#4456,.T.);
#6202=ORIENTED_EDGE('',*,*,#4457,.F.);
#6203=ORIENTED_EDGE('',*,*,#4458,.T.);
#6204=ORIENTED_EDGE('',*,*,#4459,.T.);
#6205=ORIENTED_EDGE('',*,*,#4433,.T.);
#6206=ORIENTED_EDGE('',*,*,#4460,.T.);
#6207=ORIENTED_EDGE('',*,*,#4457,.T.);
#6208=ORIENTED_EDGE('',*,*,#4441,.T.);
#6209=ORIENTED_EDGE('',*,*,#4461,.T.);
#6210=ORIENTED_EDGE('',*,*,#4462,.T.);
#6211=ORIENTED_EDGE('',*,*,#4463,.F.);
#6212=ORIENTED_EDGE('',*,*,#4464,.F.);
#6213=ORIENTED_EDGE('',*,*,#4438,.T.);
#6214=ORIENTED_EDGE('',*,*,#4465,.F.);
#6215=ORIENTED_EDGE('',*,*,#4436,.T.);
#6216=ORIENTED_EDGE('',*,*,#4437,.T.);
#6217=ORIENTED_EDGE('',*,*,#4465,.T.);
#6218=ORIENTED_EDGE('',*,*,#4466,.F.);
#6219=ORIENTED_EDGE('',*,*,#4467,.T.);
#6220=ORIENTED_EDGE('',*,*,#4458,.F.);
#6221=ORIENTED_EDGE('',*,*,#4468,.F.);
#6222=ORIENTED_EDGE('',*,*,#4469,.F.);
#6223=ORIENTED_EDGE('',*,*,#4470,.T.);
#6224=ORIENTED_EDGE('',*,*,#4406,.T.);
#6225=ORIENTED_EDGE('',*,*,#4462,.F.);
#6226=ORIENTED_EDGE('',*,*,#4471,.T.);
#6227=ORIENTED_EDGE('',*,*,#4472,.F.);
#6228=ORIENTED_EDGE('',*,*,#4473,.F.);
#6229=ORIENTED_EDGE('',*,*,#4474,.F.);
#6230=ORIENTED_EDGE('',*,*,#4475,.F.);
#6231=ORIENTED_EDGE('',*,*,#4412,.T.);
#6232=ORIENTED_EDGE('',*,*,#4463,.T.);
#6233=ORIENTED_EDGE('',*,*,#4475,.T.);
#6234=ORIENTED_EDGE('',*,*,#4476,.F.);
#6235=ORIENTED_EDGE('',*,*,#4468,.T.);
#6236=ORIENTED_EDGE('',*,*,#4477,.F.);
#6237=ORIENTED_EDGE('',*,*,#4478,.T.);
#6238=ORIENTED_EDGE('',*,*,#4479,.T.);
#6239=ORIENTED_EDGE('',*,*,#4480,.F.);
#6240=ORIENTED_EDGE('',*,*,#4456,.F.);
#6241=ORIENTED_EDGE('',*,*,#4481,.F.);
#6242=ORIENTED_EDGE('',*,*,#4482,.T.);
#6243=ORIENTED_EDGE('',*,*,#4483,.T.);
#6244=ORIENTED_EDGE('',*,*,#4484,.F.);
#6245=ORIENTED_EDGE('',*,*,#4442,.F.);
#6246=ORIENTED_EDGE('',*,*,#4480,.T.);
#6247=ORIENTED_EDGE('',*,*,#4485,.F.);
#6248=ORIENTED_EDGE('',*,*,#4486,.T.);
#6249=ORIENTED_EDGE('',*,*,#4426,.F.);
#6250=ORIENTED_EDGE('',*,*,#4443,.F.);
#6251=ORIENTED_EDGE('',*,*,#4484,.T.);
#6252=ORIENTED_EDGE('',*,*,#4487,.T.);
#6253=ORIENTED_EDGE('',*,*,#4488,.F.);
#6254=ORIENTED_EDGE('',*,*,#4489,.F.);
#6255=ORIENTED_EDGE('',*,*,#4490,.T.);
#6256=ORIENTED_EDGE('',*,*,#4452,.F.);
#6257=ORIENTED_EDGE('',*,*,#4491,.T.);
#6258=ORIENTED_EDGE('',*,*,#4492,.T.);
#6259=ORIENTED_EDGE('',*,*,#4478,.F.);
#6260=ORIENTED_EDGE('',*,*,#4493,.F.);
#6261=ORIENTED_EDGE('',*,*,#4444,.F.);
#6262=ORIENTED_EDGE('',*,*,#4488,.T.);
#6263=ORIENTED_EDGE('',*,*,#4427,.F.);
#6264=ORIENTED_EDGE('',*,*,#4477,.T.);
#6265=ORIENTED_EDGE('',*,*,#4460,.F.);
#6266=ORIENTED_EDGE('',*,*,#4493,.T.);
#6267=ORIENTED_EDGE('',*,*,#4450,.T.);
#6268=ORIENTED_EDGE('',*,*,#4421,.T.);
#6269=ORIENTED_EDGE('',*,*,#4494,.T.);
#6270=ORIENTED_EDGE('',*,*,#4495,.T.);
#6271=ORIENTED_EDGE('',*,*,#4485,.T.);
#6272=ORIENTED_EDGE('',*,*,#4479,.F.);
#6273=ORIENTED_EDGE('',*,*,#4492,.F.);
#6274=ORIENTED_EDGE('',*,*,#4496,.T.);
#6275=ORIENTED_EDGE('',*,*,#4497,.T.);
#6276=ORIENTED_EDGE('',*,*,#4417,.T.);
#6277=ORIENTED_EDGE('',*,*,#4447,.T.);
#6278=ORIENTED_EDGE('',*,*,#4498,.T.);
#6279=ORIENTED_EDGE('',*,*,#4499,.F.);
#6280=ORIENTED_EDGE('',*,*,#4419,.T.);
#6281=ORIENTED_EDGE('',*,*,#4500,.F.);
#6282=ORIENTED_EDGE('',*,*,#4501,.T.);
#6283=ORIENTED_EDGE('',*,*,#4489,.T.);
#6284=ORIENTED_EDGE('',*,*,#4487,.F.);
#6285=ORIENTED_EDGE('',*,*,#4483,.F.);
#6286=ORIENTED_EDGE('',*,*,#4502,.T.);
#6287=ORIENTED_EDGE('',*,*,#4503,.F.);
#6288=ORIENTED_EDGE('',*,*,#4504,.T.);
#6289=ORIENTED_EDGE('',*,*,#4481,.T.);
#6290=ORIENTED_EDGE('',*,*,#4505,.T.);
#6291=ORIENTED_EDGE('',*,*,#4506,.T.);
#6292=ORIENTED_EDGE('',*,*,#4423,.T.);
#6293=ORIENTED_EDGE('',*,*,#4449,.F.);
#6294=ORIENTED_EDGE('',*,*,#4500,.T.);
#6295=ORIENTED_EDGE('',*,*,#4418,.F.);
#6296=ORIENTED_EDGE('',*,*,#4497,.F.);
#6297=ORIENTED_EDGE('',*,*,#4507,.T.);
#6298=ORIENTED_EDGE('',*,*,#4454,.T.);
#6299=ORIENTED_EDGE('',*,*,#4508,.T.);
#6300=ORIENTED_EDGE('',*,*,#4432,.F.);
#6301=ORIENTED_EDGE('',*,*,#4494,.F.);
#6302=ORIENTED_EDGE('',*,*,#4420,.T.);
#6303=ORIENTED_EDGE('',*,*,#4499,.T.);
#6304=ORIENTED_EDGE('',*,*,#4509,.T.);
#6305=ORIENTED_EDGE('',*,*,#4503,.T.);
#6306=ORIENTED_EDGE('',*,*,#4510,.T.);
#6307=ORIENTED_EDGE('',*,*,#4430,.F.);
#6308=ORIENTED_EDGE('',*,*,#4429,.T.);
#6309=ORIENTED_EDGE('',*,*,#4424,.F.);
#6310=ORIENTED_EDGE('',*,*,#4509,.F.);
#6311=ORIENTED_EDGE('',*,*,#4502,.F.);
#6312=ORIENTED_EDGE('',*,*,#4482,.F.);
#6313=ORIENTED_EDGE('',*,*,#4504,.F.);
#6314=ORIENTED_EDGE('',*,*,#4490,.F.);
#6315=ORIENTED_EDGE('',*,*,#4501,.F.);
#6316=ORIENTED_EDGE('',*,*,#4508,.F.);
#6317=ORIENTED_EDGE('',*,*,#4453,.F.);
#6318=ORIENTED_EDGE('',*,*,#4507,.F.);
#6319=ORIENTED_EDGE('',*,*,#4496,.F.);
#6320=ORIENTED_EDGE('',*,*,#4491,.F.);
#6321=ORIENTED_EDGE('',*,*,#4455,.F.);
#6322=ORIENTED_EDGE('',*,*,#4486,.F.);
#6323=ORIENTED_EDGE('',*,*,#4495,.F.);
#6324=ORIENTED_EDGE('',*,*,#4510,.F.);
#6325=ORIENTED_EDGE('',*,*,#4505,.F.);
#6326=ORIENTED_EDGE('',*,*,#4414,.F.);
#6327=ORIENTED_EDGE('',*,*,#4506,.F.);
#6328=ORIENTED_EDGE('',*,*,#4451,.F.);
#6329=ORIENTED_EDGE('',*,*,#4498,.F.);
#6330=ORIENTED_EDGE('',*,*,#4448,.F.);
#6331=ORIENTED_EDGE('',*,*,#4446,.F.);
#6332=ORIENTED_EDGE('',*,*,#4435,.F.);
#6333=ORIENTED_EDGE('',*,*,#4511,.T.);
#6334=ORIENTED_EDGE('',*,*,#4466,.T.);
#6335=ORIENTED_EDGE('',*,*,#4512,.T.);
#6336=ORIENTED_EDGE('',*,*,#4472,.T.);
#6337=ORIENTED_EDGE('',*,*,#4513,.T.);
#6338=ORIENTED_EDGE('',*,*,#4439,.F.);
#6339=ORIENTED_EDGE('',*,*,#4464,.T.);
#6340=ORIENTED_EDGE('',*,*,#4512,.F.);
#6341=ORIENTED_EDGE('',*,*,#4470,.F.);
#6342=ORIENTED_EDGE('',*,*,#4514,.F.);
#6343=ORIENTED_EDGE('',*,*,#4473,.T.);
#6344=ORIENTED_EDGE('',*,*,#4474,.T.);
#6345=ORIENTED_EDGE('',*,*,#4514,.T.);
#6346=ORIENTED_EDGE('',*,*,#4469,.T.);
#6347=ORIENTED_EDGE('',*,*,#4476,.T.);
#6348=ORIENTED_EDGE('',*,*,#4434,.F.);
#6349=ORIENTED_EDGE('',*,*,#4459,.F.);
#6350=ORIENTED_EDGE('',*,*,#4467,.F.);
#6351=ORIENTED_EDGE('',*,*,#4511,.F.);
#6352=ORIENTED_EDGE('',*,*,#4471,.F.);
#6353=ORIENTED_EDGE('',*,*,#4461,.F.);
#6354=ORIENTED_EDGE('',*,*,#4440,.F.);
#6355=ORIENTED_EDGE('',*,*,#4513,.F.);
#6356=ORIENTED_EDGE('',*,*,#4515,.F.);
#6357=ORIENTED_EDGE('',*,*,#4516,.T.);
#6358=ORIENTED_EDGE('',*,*,#4516,.F.);
#6359=ORIENTED_EDGE('',*,*,#4517,.F.);
#6360=ORIENTED_EDGE('',*,*,#4518,.T.);
#6361=ORIENTED_EDGE('',*,*,#4515,.T.);
#6362=ORIENTED_EDGE('',*,*,#4518,.F.);
#6363=ORIENTED_EDGE('',*,*,#4517,.T.);
#6364=ORIENTED_EDGE('',*,*,#4519,.F.);
#6365=ORIENTED_EDGE('',*,*,#4520,.T.);
#6366=ORIENTED_EDGE('',*,*,#4521,.T.);
#6367=ORIENTED_EDGE('',*,*,#4520,.F.);
#6368=ORIENTED_EDGE('',*,*,#4522,.F.);
#6369=ORIENTED_EDGE('',*,*,#4523,.T.);
#6370=ORIENTED_EDGE('',*,*,#4524,.T.);
#6371=ORIENTED_EDGE('',*,*,#4523,.F.);
#6372=ORIENTED_EDGE('',*,*,#4525,.T.);
#6373=ORIENTED_EDGE('',*,*,#4526,.T.);
#6374=ORIENTED_EDGE('',*,*,#4527,.F.);
#6375=ORIENTED_EDGE('',*,*,#4526,.F.);
#6376=ORIENTED_EDGE('',*,*,#4525,.F.);
#6377=ORIENTED_EDGE('',*,*,#4528,.F.);
#6378=ORIENTED_EDGE('',*,*,#4529,.F.);
#6379=ORIENTED_EDGE('',*,*,#4530,.F.);
#6380=ORIENTED_EDGE('',*,*,#4531,.F.);
#6381=ORIENTED_EDGE('',*,*,#4527,.T.);
#6382=ORIENTED_EDGE('',*,*,#4521,.F.);
#6383=ORIENTED_EDGE('',*,*,#4532,.T.);
#6384=ORIENTED_EDGE('',*,*,#4533,.T.);
#6385=ORIENTED_EDGE('',*,*,#4528,.T.);
#6386=ORIENTED_EDGE('',*,*,#4534,.F.);
#6387=ORIENTED_EDGE('',*,*,#4522,.T.);
#6388=ORIENTED_EDGE('',*,*,#4535,.F.);
#6389=ORIENTED_EDGE('',*,*,#4536,.T.);
#6390=ORIENTED_EDGE('',*,*,#4534,.T.);
#6391=ORIENTED_EDGE('',*,*,#4531,.T.);
#6392=ORIENTED_EDGE('',*,*,#4537,.F.);
#6393=ORIENTED_EDGE('',*,*,#4538,.T.);
#6394=ORIENTED_EDGE('',*,*,#4535,.T.);
#6395=ORIENTED_EDGE('',*,*,#4530,.T.);
#6396=ORIENTED_EDGE('',*,*,#4524,.F.);
#6397=ORIENTED_EDGE('',*,*,#4533,.F.);
#6398=ORIENTED_EDGE('',*,*,#4539,.T.);
#6399=ORIENTED_EDGE('',*,*,#4537,.T.);
#6400=ORIENTED_EDGE('',*,*,#4529,.T.);
#6401=ORIENTED_EDGE('',*,*,#4536,.F.);
#6402=ORIENTED_EDGE('',*,*,#4538,.F.);
#6403=ORIENTED_EDGE('',*,*,#4539,.F.);
#6404=ORIENTED_EDGE('',*,*,#4532,.F.);
#6405=ORIENTED_EDGE('',*,*,#4519,.T.);
#6406=ORIENTED_EDGE('',*,*,#4540,.F.);
#6407=ORIENTED_EDGE('',*,*,#4541,.T.);
#6408=ORIENTED_EDGE('',*,*,#4542,.T.);
#6409=ORIENTED_EDGE('',*,*,#4541,.F.);
#6410=ORIENTED_EDGE('',*,*,#4543,.F.);
#6411=ORIENTED_EDGE('',*,*,#4544,.F.);
#6412=ORIENTED_EDGE('',*,*,#4545,.F.);
#6413=ORIENTED_EDGE('',*,*,#4546,.F.);
#6414=ORIENTED_EDGE('',*,*,#4547,.T.);
#6415=ORIENTED_EDGE('',*,*,#4548,.T.);
#6416=ORIENTED_EDGE('',*,*,#4549,.F.);
#6417=ORIENTED_EDGE('',*,*,#4548,.F.);
#6418=ORIENTED_EDGE('',*,*,#4549,.T.);
#6419=ORIENTED_EDGE('',*,*,#4550,.F.);
#6420=ORIENTED_EDGE('',*,*,#4551,.F.);
#6421=ORIENTED_EDGE('',*,*,#4552,.F.);
#6422=ORIENTED_EDGE('',*,*,#4553,.F.);
#6423=ORIENTED_EDGE('',*,*,#4547,.F.);
#6424=ORIENTED_EDGE('',*,*,#4554,.F.);
#6425=ORIENTED_EDGE('',*,*,#4545,.T.);
#6426=ORIENTED_EDGE('',*,*,#4555,.T.);
#6427=ORIENTED_EDGE('',*,*,#4551,.T.);
#6428=ORIENTED_EDGE('',*,*,#4542,.F.);
#6429=ORIENTED_EDGE('',*,*,#4556,.F.);
#6430=ORIENTED_EDGE('',*,*,#4546,.T.);
#6431=ORIENTED_EDGE('',*,*,#4554,.T.);
#6432=ORIENTED_EDGE('',*,*,#4550,.T.);
#6433=ORIENTED_EDGE('',*,*,#4543,.T.);
#6434=ORIENTED_EDGE('',*,*,#4556,.T.);
#6435=ORIENTED_EDGE('',*,*,#4553,.T.);
#6436=ORIENTED_EDGE('',*,*,#4557,.F.);
#6437=ORIENTED_EDGE('',*,*,#4540,.T.);
#6438=ORIENTED_EDGE('',*,*,#4555,.F.);
#6439=ORIENTED_EDGE('',*,*,#4544,.T.);
#6440=ORIENTED_EDGE('',*,*,#4557,.T.);
#6441=ORIENTED_EDGE('',*,*,#4552,.T.);
#6442=TOROIDAL_SURFACE('',#7062,22.,2.);
#6443=TOROIDAL_SURFACE('',#7067,22.,2.);
#6444=TOROIDAL_SURFACE('',#7159,54.4897440054506,2.);
#6445=TOROIDAL_SURFACE('',#7161,161.25688730188,2.);
#6446=TOROIDAL_SURFACE('',#7169,4.,2.);
#6447=TOROIDAL_SURFACE('',#7181,161.25688730188,2.);
#6448=TOROIDAL_SURFACE('',#7183,4.,2.);
#6449=TOROIDAL_SURFACE('',#7186,54.4897440054506,2.);
#6450=TOROIDAL_SURFACE('',#7358,9.44563594905814,2.);
#6451=TOROIDAL_SURFACE('',#7384,8.16998586739121,2.);
#6452=ADVANCED_FACE('',(#1800),#6442,.T.);
#6453=ADVANCED_FACE('',(#1801),#6443,.T.);
#6454=ADVANCED_FACE('',(#1802),#1789,.T.);
#6455=ADVANCED_FACE('',(#1803),#1646,.F.);
#6456=ADVANCED_FACE('',(#1804),#1647,.F.);
#6457=ADVANCED_FACE('',(#1805),#1648,.T.);
#6458=ADVANCED_FACE('',(#1806),#397,.T.);
#6459=ADVANCED_FACE('',(#1807,#284),#398,.T.);
#6460=ADVANCED_FACE('',(#1808),#399,.T.);
#6461=ADVANCED_FACE('',(#1809,#285),#400,.T.);
#6462=ADVANCED_FACE('',(#1810,#286),#1649,.T.);
#6463=ADVANCED_FACE('',(#1811),#401,.T.);
#6464=ADVANCED_FACE('',(#1812,#287),#1650,.F.);
#6465=ADVANCED_FACE('',(#1813),#402,.F.);
#6466=ADVANCED_FACE('',(#1814),#403,.F.);
#6467=ADVANCED_FACE('',(#1815),#404,.F.);
#6468=ADVANCED_FACE('',(#1816),#405,.F.);
#6469=ADVANCED_FACE('',(#1817),#406,.T.);
#6470=ADVANCED_FACE('',(#1818),#407,.F.);
#6471=ADVANCED_FACE('',(#1819,#288),#408,.T.);
#6472=ADVANCED_FACE('',(#1820,#289),#409,.F.);
#6473=ADVANCED_FACE('',(#1821),#410,.F.);
#6474=ADVANCED_FACE('',(#1822),#411,.F.);
#6475=ADVANCED_FACE('',(#1823),#1651,.T.);
#6476=ADVANCED_FACE('',(#1824),#412,.F.);
#6477=ADVANCED_FACE('',(#1825),#413,.T.);
#6478=ADVANCED_FACE('',(#1826),#1652,.T.);
#6479=ADVANCED_FACE('',(#1827),#1790,.T.);
#6480=ADVANCED_FACE('',(#1828),#1791,.T.);
#6481=ADVANCED_FACE('',(#1829),#1653,.T.);
#6482=ADVANCED_FACE('',(#1830),#1654,.T.);
#6483=ADVANCED_FACE('',(#1831),#1655,.T.);
#6484=ADVANCED_FACE('',(#1832),#1656,.T.);
#6485=ADVANCED_FACE('',(#1833),#1657,.T.);
#6486=ADVANCED_FACE('',(#1834),#1792,.T.);
#6487=ADVANCED_FACE('',(#1835),#1793,.T.);
#6488=ADVANCED_FACE('',(#1836),#1794,.T.);
#6489=ADVANCED_FACE('',(#1837),#1658,.T.);
#6490=ADVANCED_FACE('',(#1838),#1659,.T.);
#6491=ADVANCED_FACE('',(#1839),#1660,.T.);
#6492=ADVANCED_FACE('',(#1840),#6444,.T.);
#6493=ADVANCED_FACE('',(#1841),#6445,.T.);
#6494=ADVANCED_FACE('',(#1842),#1661,.T.);
#6495=ADVANCED_FACE('',(#1843),#1662,.T.);
#6496=ADVANCED_FACE('',(#1844),#1795,.T.);
#6497=ADVANCED_FACE('',(#1845),#6446,.T.);
#6498=ADVANCED_FACE('',(#1846),#1796,.T.);
#6499=ADVANCED_FACE('',(#1847),#1797,.T.);
#6500=ADVANCED_FACE('',(#1848),#1663,.T.);
#6501=ADVANCED_FACE('',(#1849),#1664,.F.);
#6502=ADVANCED_FACE('',(#1850),#1665,.T.);
#6503=ADVANCED_FACE('',(#1851),#6447,.T.);
#6504=ADVANCED_FACE('',(#1852),#6448,.T.);
#6505=ADVANCED_FACE('',(#1853),#1798,.T.);
#6506=ADVANCED_FACE('',(#1854),#6449,.T.);
#6507=ADVANCED_FACE('',(#1855),#1666,.T.);
#6508=ADVANCED_FACE('',(#1856),#414,.T.);
#6509=ADVANCED_FACE('',(#1857),#415,.T.);
#6510=ADVANCED_FACE('',(#1858),#1667,.T.);
#6511=ADVANCED_FACE('',(#1859),#1668,.T.);
#6512=ADVANCED_FACE('',(#1860),#1669,.F.);
#6513=ADVANCED_FACE('',(#1861),#1670,.F.);
#6514=ADVANCED_FACE('',(#1862),#1671,.T.);
#6515=ADVANCED_FACE('',(#1863),#1672,.T.);
#6516=ADVANCED_FACE('',(#1864),#1673,.T.);
#6517=ADVANCED_FACE('',(#1865),#1674,.F.);
#6518=ADVANCED_FACE('',(#1866),#1675,.F.);
#6519=ADVANCED_FACE('',(#1867,#290,#291),#117,.T.);
#6520=ADVANCED_FACE('',(#1868),#416,.F.);
#6521=ADVANCED_FACE('',(#1869),#417,.F.);
#6522=ADVANCED_FACE('',(#1870),#418,.F.);
#6523=ADVANCED_FACE('',(#1871),#419,.T.);
#6524=ADVANCED_FACE('',(#1872),#118,.T.);
#6525=ADVANCED_FACE('',(#1873),#1676,.F.);
#6526=ADVANCED_FACE('',(#1874,#292),#1677,.T.);
#6527=ADVANCED_FACE('',(#1875),#420,.T.);
#6528=ADVANCED_FACE('',(#1876,#293),#421,.T.);
#6529=ADVANCED_FACE('',(#1877,#294),#422,.T.);
#6530=ADVANCED_FACE('',(#1878),#423,.F.);
#6531=ADVANCED_FACE('',(#1879),#424,.F.);
#6532=ADVANCED_FACE('',(#1880,#295),#425,.F.);
#6533=ADVANCED_FACE('',(#1881),#426,.F.);
#6534=ADVANCED_FACE('',(#1882,#296),#427,.F.);
#6535=ADVANCED_FACE('',(#1883),#428,.F.);
#6536=ADVANCED_FACE('',(#1884),#429,.F.);
#6537=ADVANCED_FACE('',(#1885),#430,.T.);
#6538=ADVANCED_FACE('',(#1886),#431,.F.);
#6539=ADVANCED_FACE('',(#1887,#297),#432,.F.);
#6540=ADVANCED_FACE('',(#1888,#298),#433,.F.);
#6541=ADVANCED_FACE('',(#1889),#434,.T.);
#6542=ADVANCED_FACE('',(#1890),#435,.F.);
#6543=ADVANCED_FACE('',(#1891),#1678,.T.);
#6544=ADVANCED_FACE('',(#1892),#1679,.T.);
#6545=ADVANCED_FACE('',(#1893),#1680,.T.);
#6546=ADVANCED_FACE('',(#1894),#1681,.T.);
#6547=ADVANCED_FACE('',(#1895),#1682,.T.);
#6548=ADVANCED_FACE('',(#1896),#436,.F.);
#6549=ADVANCED_FACE('',(#1897,#299),#437,.T.);
#6550=ADVANCED_FACE('',(#1898),#438,.T.);
#6551=ADVANCED_FACE('',(#1899,#300),#439,.T.);
#6552=ADVANCED_FACE('',(#1900),#440,.T.);
#6553=ADVANCED_FACE('',(#1901),#1683,.T.);
#6554=ADVANCED_FACE('',(#1902),#1684,.T.);
#6555=ADVANCED_FACE('',(#1903),#1685,.F.);
#6556=ADVANCED_FACE('',(#1904),#1686,.T.);
#6557=ADVANCED_FACE('',(#1905),#1687,.T.);
#6558=ADVANCED_FACE('',(#1906),#1688,.T.);
#6559=ADVANCED_FACE('',(#1907),#1689,.F.);
#6560=ADVANCED_FACE('',(#1908),#1690,.F.);
#6561=ADVANCED_FACE('',(#1909,#301,#302),#119,.T.);
#6562=ADVANCED_FACE('',(#1910),#1691,.F.);
#6563=ADVANCED_FACE('',(#1911),#441,.T.);
#6564=ADVANCED_FACE('',(#1912),#120,.T.);
#6565=ADVANCED_FACE('',(#1913,#303),#1692,.T.);
#6566=ADVANCED_FACE('',(#1914),#442,.T.);
#6567=ADVANCED_FACE('',(#1915,#304),#443,.T.);
#6568=ADVANCED_FACE('',(#1916,#305),#444,.T.);
#6569=ADVANCED_FACE('',(#1917),#445,.F.);
#6570=ADVANCED_FACE('',(#1918),#446,.F.);
#6571=ADVANCED_FACE('',(#1919,#306),#447,.F.);
#6572=ADVANCED_FACE('',(#1920),#448,.F.);
#6573=ADVANCED_FACE('',(#1921,#307),#449,.F.);
#6574=ADVANCED_FACE('',(#1922),#450,.F.);
#6575=ADVANCED_FACE('',(#1923),#451,.F.);
#6576=ADVANCED_FACE('',(#1924),#452,.T.);
#6577=ADVANCED_FACE('',(#1925),#453,.F.);
#6578=ADVANCED_FACE('',(#1926,#308),#454,.F.);
#6579=ADVANCED_FACE('',(#1927,#309),#455,.F.);
#6580=ADVANCED_FACE('',(#1928),#456,.T.);
#6581=ADVANCED_FACE('',(#1929),#457,.F.);
#6582=ADVANCED_FACE('',(#1930),#1693,.T.);
#6583=ADVANCED_FACE('',(#1931),#1694,.T.);
#6584=ADVANCED_FACE('',(#1932),#1695,.T.);
#6585=ADVANCED_FACE('',(#1933),#1696,.T.);
#6586=ADVANCED_FACE('',(#1934),#1697,.T.);
#6587=ADVANCED_FACE('',(#1935),#1698,.T.);
#6588=ADVANCED_FACE('',(#1936),#458,.F.);
#6589=ADVANCED_FACE('',(#1937,#310),#459,.T.);
#6590=ADVANCED_FACE('',(#1938),#460,.T.);
#6591=ADVANCED_FACE('',(#1939,#311),#461,.T.);
#6592=ADVANCED_FACE('',(#1940),#462,.T.);
#6593=ADVANCED_FACE('',(#1941),#1699,.T.);
#6594=ADVANCED_FACE('',(#1942),#1700,.T.);
#6595=ADVANCED_FACE('',(#1943),#1701,.F.);
#6596=ADVANCED_FACE('',(#1944),#1702,.F.);
#6597=ADVANCED_FACE('',(#1945),#1703,.T.);
#6598=ADVANCED_FACE('',(#1946),#1704,.T.);
#6599=ADVANCED_FACE('',(#1947),#6450,.T.);
#6600=ADVANCED_FACE('',(#1948),#1705,.F.);
#6601=ADVANCED_FACE('',(#1949),#1706,.T.);
#6602=ADVANCED_FACE('',(#1950),#1707,.T.);
#6603=ADVANCED_FACE('',(#1951),#1708,.T.);
#6604=ADVANCED_FACE('',(#1952),#1709,.F.);
#6605=ADVANCED_FACE('',(#1953),#1710,.F.);
#6606=ADVANCED_FACE('',(#1954,#312,#313),#121,.T.);
#6607=ADVANCED_FACE('',(#1955),#1711,.F.);
#6608=ADVANCED_FACE('',(#1956),#1712,.F.);
#6609=ADVANCED_FACE('',(#1957,#314),#6451,.T.);
#6610=ADVANCED_FACE('',(#1958),#1713,.F.);
#6611=ADVANCED_FACE('',(#1959),#463,.T.);
#6612=ADVANCED_FACE('',(#1960),#122,.T.);
#6613=ADVANCED_FACE('',(#1961,#315),#1714,.T.);
#6614=ADVANCED_FACE('',(#1962),#464,.T.);
#6615=ADVANCED_FACE('',(#1963,#316),#465,.T.);
#6616=ADVANCED_FACE('',(#1964,#317),#466,.T.);
#6617=ADVANCED_FACE('',(#1965),#467,.F.);
#6618=ADVANCED_FACE('',(#1966),#468,.F.);
#6619=ADVANCED_FACE('',(#1967,#318),#469,.F.);
#6620=ADVANCED_FACE('',(#1968),#470,.F.);
#6621=ADVANCED_FACE('',(#1969,#319),#471,.F.);
#6622=ADVANCED_FACE('',(#1970),#472,.F.);
#6623=ADVANCED_FACE('',(#1971),#473,.F.);
#6624=ADVANCED_FACE('',(#1972),#474,.T.);
#6625=ADVANCED_FACE('',(#1973),#475,.F.);
#6626=ADVANCED_FACE('',(#1974,#320),#476,.F.);
#6627=ADVANCED_FACE('',(#1975,#321),#477,.F.);
#6628=ADVANCED_FACE('',(#1976),#478,.T.);
#6629=ADVANCED_FACE('',(#1977),#479,.F.);
#6630=ADVANCED_FACE('',(#1978),#1715,.T.);
#6631=ADVANCED_FACE('',(#1979),#1716,.T.);
#6632=ADVANCED_FACE('',(#1980),#1717,.T.);
#6633=ADVANCED_FACE('',(#1981),#1718,.T.);
#6634=ADVANCED_FACE('',(#1982),#1719,.T.);
#6635=ADVANCED_FACE('',(#1983),#1720,.T.);
#6636=ADVANCED_FACE('',(#1984),#480,.F.);
#6637=ADVANCED_FACE('',(#1985,#322),#481,.T.);
#6638=ADVANCED_FACE('',(#1986),#482,.T.);
#6639=ADVANCED_FACE('',(#1987,#323),#483,.T.);
#6640=ADVANCED_FACE('',(#1988),#484,.T.);
#6641=ADVANCED_FACE('',(#1989),#1721,.T.);
#6642=ADVANCED_FACE('',(#1990),#1722,.T.);
#6643=ADVANCED_FACE('',(#1991),#1723,.T.);
#6644=ADVANCED_FACE('',(#1992),#1724,.T.);
#6645=ADVANCED_FACE('',(#1993),#1725,.F.);
#6646=ADVANCED_FACE('',(#1994),#1726,.F.);
#6647=ADVANCED_FACE('',(#1995),#1727,.F.);
#6648=ADVANCED_FACE('',(#1996),#1728,.T.);
#6649=ADVANCED_FACE('',(#1997),#1729,.T.);
#6650=ADVANCED_FACE('',(#1998),#1730,.F.);
#6651=ADVANCED_FACE('',(#1999),#1731,.F.);
#6652=ADVANCED_FACE('',(#2000),#1732,.T.);
#6653=ADVANCED_FACE('',(#2001,#324),#485,.F.);
#6654=ADVANCED_FACE('',(#2002,#325),#486,.T.);
#6655=ADVANCED_FACE('',(#2003,#326),#487,.F.);
#6656=ADVANCED_FACE('',(#2004),#488,.F.);
#6657=ADVANCED_FACE('',(#2005,#327),#489,.F.);
#6658=ADVANCED_FACE('',(#2006),#490,.F.);
#6659=ADVANCED_FACE('',(#2007),#1733,.T.);
#6660=ADVANCED_FACE('',(#2008),#491,.T.);
#6661=ADVANCED_FACE('',(#2009),#1734,.F.);
#6662=ADVANCED_FACE('',(#2010),#1735,.T.);
#6663=ADVANCED_FACE('',(#2011),#1736,.T.);
#6664=ADVANCED_FACE('',(#2012,#328),#492,.T.);
#6665=ADVANCED_FACE('',(#2013),#493,.F.);
#6666=ADVANCED_FACE('',(#2014,#329),#494,.F.);
#6667=ADVANCED_FACE('',(#2015),#495,.F.);
#6668=ADVANCED_FACE('',(#2016,#330),#496,.F.);
#6669=ADVANCED_FACE('',(#2017),#497,.F.);
#6670=ADVANCED_FACE('',(#2018),#1737,.F.);
#6671=ADVANCED_FACE('',(#2019),#1738,.F.);
#6672=ADVANCED_FACE('',(#2020),#1739,.T.);
#6673=ADVANCED_FACE('',(#2021,#331),#498,.F.);
#6674=ADVANCED_FACE('',(#2022,#332),#499,.T.);
#6675=ADVANCED_FACE('',(#2023,#333),#500,.F.);
#6676=ADVANCED_FACE('',(#2024),#501,.F.);
#6677=ADVANCED_FACE('',(#2025,#334),#502,.F.);
#6678=ADVANCED_FACE('',(#2026),#503,.F.);
#6679=ADVANCED_FACE('',(#2027),#1740,.T.);
#6680=ADVANCED_FACE('',(#2028),#504,.T.);
#6681=ADVANCED_FACE('',(#2029),#1741,.F.);
#6682=ADVANCED_FACE('',(#2030),#1742,.T.);
#6683=ADVANCED_FACE('',(#2031),#1743,.T.);
#6684=ADVANCED_FACE('',(#2032,#335),#505,.T.);
#6685=ADVANCED_FACE('',(#2033),#506,.F.);
#6686=ADVANCED_FACE('',(#2034,#336),#507,.F.);
#6687=ADVANCED_FACE('',(#2035),#508,.F.);
#6688=ADVANCED_FACE('',(#2036,#337),#509,.F.);
#6689=ADVANCED_FACE('',(#2037),#510,.F.);
#6690=ADVANCED_FACE('',(#2038),#1744,.F.);
#6691=ADVANCED_FACE('',(#2039),#1745,.F.);
#6692=ADVANCED_FACE('',(#2040),#1746,.T.);
#6693=ADVANCED_FACE('',(#2041,#338),#511,.F.);
#6694=ADVANCED_FACE('',(#2042,#339),#512,.T.);
#6695=ADVANCED_FACE('',(#2043,#340),#513,.F.);
#6696=ADVANCED_FACE('',(#2044),#514,.F.);
#6697=ADVANCED_FACE('',(#2045,#341),#515,.F.);
#6698=ADVANCED_FACE('',(#2046),#516,.F.);
#6699=ADVANCED_FACE('',(#2047),#1747,.T.);
#6700=ADVANCED_FACE('',(#2048),#517,.T.);
#6701=ADVANCED_FACE('',(#2049),#1748,.F.);
#6702=ADVANCED_FACE('',(#2050),#1749,.T.);
#6703=ADVANCED_FACE('',(#2051),#1750,.T.);
#6704=ADVANCED_FACE('',(#2052,#342),#518,.T.);
#6705=ADVANCED_FACE('',(#2053),#519,.F.);
#6706=ADVANCED_FACE('',(#2054,#343),#520,.F.);
#6707=ADVANCED_FACE('',(#2055),#521,.F.);
#6708=ADVANCED_FACE('',(#2056,#344),#522,.F.);
#6709=ADVANCED_FACE('',(#2057),#523,.F.);
#6710=ADVANCED_FACE('',(#2058),#1751,.T.);
#6711=ADVANCED_FACE('',(#2059),#1752,.T.);
#6712=ADVANCED_FACE('',(#2060),#1753,.T.);
#6713=ADVANCED_FACE('',(#2061),#524,.T.);
#6714=ADVANCED_FACE('',(#2062,#345),#525,.F.);
#6715=ADVANCED_FACE('',(#2063),#526,.F.);
#6716=ADVANCED_FACE('',(#2064,#346),#527,.F.);
#6717=ADVANCED_FACE('',(#2065),#528,.F.);
#6718=ADVANCED_FACE('',(#2066),#529,.T.);
#6719=ADVANCED_FACE('',(#2067),#530,.F.);
#6720=ADVANCED_FACE('',(#2068),#531,.F.);
#6721=ADVANCED_FACE('',(#2069),#532,.T.);
#6722=ADVANCED_FACE('',(#2070,#347),#533,.F.);
#6723=ADVANCED_FACE('',(#2071,#348),#534,.F.);
#6724=ADVANCED_FACE('',(#2072),#535,.F.);
#6725=ADVANCED_FACE('',(#2073),#536,.F.);
#6726=ADVANCED_FACE('',(#2074),#537,.T.);
#6727=ADVANCED_FACE('',(#2075),#1754,.F.);
#6728=ADVANCED_FACE('',(#2076),#1755,.F.);
#6729=ADVANCED_FACE('',(#2077),#17,.F.);
#6730=ADVANCED_FACE('',(#2078,#349,#350),#18,.F.);
#6731=ADVANCED_FACE('',(#2079,#351),#1756,.F.);
#6732=ADVANCED_FACE('',(#2080),#538,.T.);
#6733=ADVANCED_FACE('',(#2081),#539,.F.);
#6734=ADVANCED_FACE('',(#2082,#352),#540,.F.);
#6735=ADVANCED_FACE('',(#2083),#541,.F.);
#6736=ADVANCED_FACE('',(#2084,#353),#542,.F.);
#6737=ADVANCED_FACE('',(#2085),#1757,.T.);
#6738=ADVANCED_FACE('',(#2086),#1758,.F.);
#6739=ADVANCED_FACE('',(#2087),#1759,.F.);
#6740=ADVANCED_FACE('',(#2088),#1760,.F.);
#6741=ADVANCED_FACE('',(#2089,#354,#355),#1799,.T.);
#6742=ADVANCED_FACE('',(#2090),#543,.T.);
#6743=ADVANCED_FACE('',(#2091),#544,.T.);
#6744=ADVANCED_FACE('',(#2092,#356),#545,.F.);
#6745=ADVANCED_FACE('',(#2093),#546,.F.);
#6746=ADVANCED_FACE('',(#2094,#357),#547,.T.);
#6747=ADVANCED_FACE('',(#2095),#548,.F.);
#6748=ADVANCED_FACE('',(#2096,#358),#549,.T.);
#6749=ADVANCED_FACE('',(#2097),#550,.T.);
#6750=ADVANCED_FACE('',(#2098,#359),#551,.T.);
#6751=ADVANCED_FACE('',(#2099),#552,.T.);
#6752=ADVANCED_FACE('',(#2100),#553,.F.);
#6753=ADVANCED_FACE('',(#2101),#554,.F.);
#6754=ADVANCED_FACE('',(#2102),#555,.F.);
#6755=ADVANCED_FACE('',(#2103),#556,.F.);
#6756=ADVANCED_FACE('',(#2104),#557,.T.);
#6757=ADVANCED_FACE('',(#2105),#558,.F.);
#6758=ADVANCED_FACE('',(#2106,#360),#559,.F.);
#6759=ADVANCED_FACE('',(#2107,#361),#560,.F.);
#6760=ADVANCED_FACE('',(#2108),#1761,.F.);
#6761=ADVANCED_FACE('',(#2109),#1762,.F.);
#6762=ADVANCED_FACE('',(#2110),#1763,.F.);
#6763=ADVANCED_FACE('',(#2111),#561,.T.);
#6764=ADVANCED_FACE('',(#2112),#1764,.T.);
#6765=ADVANCED_FACE('',(#2113),#1765,.T.);
#6766=ADVANCED_FACE('',(#2114,#362,#363),#123,.T.);
#6767=ADVANCED_FACE('',(#2115),#562,.T.);
#6768=ADVANCED_FACE('',(#2116),#563,.T.);
#6769=ADVANCED_FACE('',(#2117),#1766,.F.);
#6770=ADVANCED_FACE('',(#2118,#364),#564,.T.);
#6771=ADVANCED_FACE('',(#2119,#365),#565,.T.);
#6772=ADVANCED_FACE('',(#2120),#566,.T.);
#6773=ADVANCED_FACE('',(#2121),#567,.F.);
#6774=ADVANCED_FACE('',(#2122),#568,.T.);
#6775=ADVANCED_FACE('',(#2123),#569,.T.);
#6776=ADVANCED_FACE('',(#2124),#570,.T.);
#6777=ADVANCED_FACE('',(#2125,#366),#571,.F.);
#6778=ADVANCED_FACE('',(#2126,#367),#572,.T.);
#6779=ADVANCED_FACE('',(#2127),#1767,.F.);
#6780=ADVANCED_FACE('',(#2128),#1768,.F.);
#6781=ADVANCED_FACE('',(#2129),#1769,.F.);
#6782=ADVANCED_FACE('',(#2130),#1770,.T.);
#6783=ADVANCED_FACE('',(#2131),#1771,.T.);
#6784=ADVANCED_FACE('',(#2132),#1772,.T.);
#6785=ADVANCED_FACE('',(#2133,#368,#369),#124,.T.);
#6786=ADVANCED_FACE('',(#2134),#573,.F.);
#6787=ADVANCED_FACE('',(#2135),#574,.F.);
#6788=ADVANCED_FACE('',(#2136),#575,.F.);
#6789=ADVANCED_FACE('',(#2137),#576,.T.);
#6790=ADVANCED_FACE('',(#2138),#125,.T.);
#6791=ADVANCED_FACE('',(#2139),#1773,.F.);
#6792=ADVANCED_FACE('',(#2140),#577,.T.);
#6793=ADVANCED_FACE('',(#2141),#578,.T.);
#6794=ADVANCED_FACE('',(#2142,#370),#579,.T.);
#6795=ADVANCED_FACE('',(#2143,#371),#580,.T.);
#6796=ADVANCED_FACE('',(#2144),#581,.F.);
#6797=ADVANCED_FACE('',(#2145),#582,.F.);
#6798=ADVANCED_FACE('',(#2146,#372),#583,.F.);
#6799=ADVANCED_FACE('',(#2147),#584,.F.);
#6800=ADVANCED_FACE('',(#2148,#373),#585,.F.);
#6801=ADVANCED_FACE('',(#2149),#126,.F.);
#6802=ADVANCED_FACE('',(#2150),#586,.F.);
#6803=ADVANCED_FACE('',(#2151),#587,.F.);
#6804=ADVANCED_FACE('',(#2152),#588,.T.);
#6805=ADVANCED_FACE('',(#2153),#589,.F.);
#6806=ADVANCED_FACE('',(#2154,#374),#590,.F.);
#6807=ADVANCED_FACE('',(#2155,#375),#591,.F.);
#6808=ADVANCED_FACE('',(#2156),#592,.T.);
#6809=ADVANCED_FACE('',(#2157),#593,.F.);
#6810=ADVANCED_FACE('',(#2158),#1774,.T.);
#6811=ADVANCED_FACE('',(#2159),#1775,.T.);
#6812=ADVANCED_FACE('',(#2160),#1776,.T.);
#6813=ADVANCED_FACE('',(#2161),#1777,.T.);
#6814=ADVANCED_FACE('',(#2162),#1778,.T.);
#6815=ADVANCED_FACE('',(#2163),#1779,.F.);
#6816=ADVANCED_FACE('',(#2164),#594,.F.);
#6817=ADVANCED_FACE('',(#2165),#595,.T.);
#6818=ADVANCED_FACE('',(#2166),#1780,.T.);
#6819=ADVANCED_FACE('',(#2167),#1781,.T.);
#6820=ADVANCED_FACE('',(#2168),#19,.F.);
#6821=ADVANCED_FACE('',(#2169),#20,.F.);
#6822=ADVANCED_FACE('',(#2170),#596,.T.);
#6823=ADVANCED_FACE('',(#2171),#1782,.F.);
#6824=ADVANCED_FACE('',(#2172),#1783,.F.);
#6825=ADVANCED_FACE('',(#2173),#1784,.T.);
#6826=ADVANCED_FACE('',(#2174,#376),#597,.F.);
#6827=ADVANCED_FACE('',(#2175,#377),#598,.T.);
#6828=ADVANCED_FACE('',(#2176,#378),#599,.F.);
#6829=ADVANCED_FACE('',(#2177),#600,.F.);
#6830=ADVANCED_FACE('',(#2178,#379),#601,.F.);
#6831=ADVANCED_FACE('',(#2179),#602,.F.);
#6832=ADVANCED_FACE('',(#2180),#1785,.T.);
#6833=ADVANCED_FACE('',(#2181),#603,.T.);
#6834=ADVANCED_FACE('',(#2182),#1786,.F.);
#6835=ADVANCED_FACE('',(#2183),#1787,.T.);
#6836=ADVANCED_FACE('',(#2184),#1788,.T.);
#6837=ADVANCED_FACE('',(#2185,#380),#604,.T.);
#6838=ADVANCED_FACE('',(#2186),#605,.F.);
#6839=ADVANCED_FACE('',(#2187,#381),#606,.F.);
#6840=ADVANCED_FACE('',(#2188),#607,.F.);
#6841=ADVANCED_FACE('',(#2189,#382),#608,.F.);
#6842=ADVANCED_FACE('',(#2190),#609,.F.);
#6843=CLOSED_SHELL('',(#6452,#6453,#6454,#6455,#6456,#6457,#6458,#6459,
#6460,#6461,#6462,#6463,#6464,#6465,#6466,#6467,#6468,#6469,#6470,#6471,
#6472,#6473,#6474,#6475,#6476,#6477,#6478,#6479,#6480,#6481,#6482,#6483,
#6484,#6485,#6486,#6487,#6488,#6489,#6490,#6491,#6492,#6493,#6494,#6495,
#6496,#6497,#6498,#6499,#6500,#6501,#6502,#6503,#6504,#6505,#6506,#6507,
#6508,#6509,#6510,#6511));
#6844=CLOSED_SHELL('',(#6512,#6513,#6514,#6515,#6516,#6517,#6518,#6519,
#6520,#6521,#6522,#6523,#6524,#6525,#6526,#6527,#6528,#6529,#6530,#6531,
#6532,#6533,#6534,#6535,#6536,#6537,#6538,#6539,#6540,#6541,#6542,#6543,
#6544,#6545,#6546,#6547,#6548,#6549,#6550,#6551,#6552,#6553,#6554));
#6845=CLOSED_SHELL('',(#6555,#6556,#6557,#6558,#6559,#6560,#6561,#6562,
#6563,#6564,#6565,#6566,#6567,#6568,#6569,#6570,#6571,#6572,#6573,#6574,
#6575,#6576,#6577,#6578,#6579,#6580,#6581,#6582,#6583,#6584,#6585,#6586,
#6587,#6588,#6589,#6590,#6591,#6592,#6593,#6594,#6595,#6596,#6597,#6598,
#6599));
#6846=CLOSED_SHELL('',(#6600,#6601,#6602,#6603,#6604,#6605,#6606,#6607,
#6608,#6609,#6610,#6611,#6612,#6613,#6614,#6615,#6616,#6617,#6618,#6619,
#6620,#6621,#6622,#6623,#6624,#6625,#6626,#6627,#6628,#6629,#6630,#6631,
#6632,#6633,#6634,#6635,#6636,#6637,#6638,#6639,#6640,#6641,#6642,#6643,
#6644,#6645,#6646,#6647,#6648,#6649));
#6847=CLOSED_SHELL('',(#6650,#6651,#6652,#6653,#6654,#6655,#6656,#6657,
#6658,#6659,#6660));
#6848=CLOSED_SHELL('',(#6661,#6662,#6663,#6664,#6665,#6666,#6667,#6668,
#6669));
#6849=CLOSED_SHELL('',(#6670,#6671,#6672,#6673,#6674,#6675,#6676,#6677,
#6678,#6679,#6680));
#6850=CLOSED_SHELL('',(#6681,#6682,#6683,#6684,#6685,#6686,#6687,#6688,
#6689));
#6851=CLOSED_SHELL('',(#6690,#6691,#6692,#6693,#6694,#6695,#6696,#6697,
#6698,#6699,#6700));
#6852=CLOSED_SHELL('',(#6701,#6702,#6703,#6704,#6705,#6706,#6707,#6708,
#6709));
#6853=CLOSED_SHELL('',(#6710,#6711,#6712,#6713,#6714,#6715,#6716,#6717,
#6718,#6719,#6720,#6721,#6722,#6723,#6724,#6725,#6726));
#6854=CLOSED_SHELL('',(#6727,#6728,#6729,#6730,#6731,#6732,#6733,#6734,
#6735,#6736));
#6855=CLOSED_SHELL('',(#6737,#6738,#6739,#6740,#6741,#6742,#6743,#6744,
#6745,#6746,#6747,#6748,#6749,#6750,#6751,#6752,#6753,#6754,#6755,#6756,
#6757,#6758,#6759));
#6856=CLOSED_SHELL('',(#6760,#6761,#6762,#6763,#6764,#6765,#6766,#6767,
#6768,#6769,#6770,#6771,#6772,#6773,#6774,#6775,#6776,#6777,#6778));
#6857=CLOSED_SHELL('',(#6779,#6780,#6781,#6782,#6783,#6784,#6785,#6786,
#6787,#6788,#6789,#6790,#6791,#6792,#6793,#6794,#6795,#6796,#6797,#6798,
#6799,#6800,#6801,#6802,#6803,#6804,#6805,#6806,#6807,#6808,#6809,#6810,
#6811,#6812,#6813,#6814,#6815,#6816,#6817,#6818,#6819));
#6858=CLOSED_SHELL('',(#6820,#6821,#6822));
#6859=CLOSED_SHELL('',(#6823,#6824,#6825,#6826,#6827,#6828,#6829,#6830,
#6831,#6832,#6833));
#6860=CLOSED_SHELL('',(#6834,#6835,#6836,#6837,#6838,#6839,#6840,#6841,
#6842));
#6861=DERIVED_UNIT_ELEMENT(#6897,1.);
#6862=DERIVED_UNIT_ELEMENT(#13201,-3.);
#6863=DERIVED_UNIT_ELEMENT(#6897,1.);
#6864=DERIVED_UNIT_ELEMENT(#13201,-3.);
#6865=DERIVED_UNIT_ELEMENT(#6897,1.);
#6866=DERIVED_UNIT_ELEMENT(#13201,-3.);
#6867=DERIVED_UNIT_ELEMENT(#6897,1.);
#6868=DERIVED_UNIT_ELEMENT(#13201,-3.);
#6869=DERIVED_UNIT_ELEMENT(#6897,1.);
#6870=DERIVED_UNIT_ELEMENT(#13201,-3.);
#6871=DERIVED_UNIT_ELEMENT(#6897,1.);
#6872=DERIVED_UNIT_ELEMENT(#13201,-3.);
#6873=DERIVED_UNIT_ELEMENT(#6897,1.);
#6874=DERIVED_UNIT_ELEMENT(#13201,-3.);
#6875=DERIVED_UNIT_ELEMENT(#6897,1.);
#6876=DERIVED_UNIT_ELEMENT(#13201,-3.);
#6877=DERIVED_UNIT_ELEMENT(#6897,1.);
#6878=DERIVED_UNIT_ELEMENT(#13201,-3.);
#6879=DERIVED_UNIT_ELEMENT(#6897,1.);
#6880=DERIVED_UNIT_ELEMENT(#13201,-3.);
#6881=DERIVED_UNIT_ELEMENT(#6897,1.);
#6882=DERIVED_UNIT_ELEMENT(#13201,-3.);
#6883=DERIVED_UNIT_ELEMENT(#6897,1.);
#6884=DERIVED_UNIT_ELEMENT(#13201,-3.);
#6885=DERIVED_UNIT_ELEMENT(#6897,1.);
#6886=DERIVED_UNIT_ELEMENT(#13201,-3.);
#6887=DERIVED_UNIT_ELEMENT(#6897,1.);
#6888=DERIVED_UNIT_ELEMENT(#13201,-3.);
#6889=DERIVED_UNIT_ELEMENT(#6897,1.);
#6890=DERIVED_UNIT_ELEMENT(#13201,-3.);
#6891=DERIVED_UNIT_ELEMENT(#6897,1.);
#6892=DERIVED_UNIT_ELEMENT(#13201,-3.);
#6893=DERIVED_UNIT_ELEMENT(#6897,1.);
#6894=DERIVED_UNIT_ELEMENT(#13201,-3.);
#6895=DERIVED_UNIT_ELEMENT(#6897,1.);
#6896=DERIVED_UNIT_ELEMENT(#13201,-3.);
#6897=(
MASS_UNIT()
NAMED_UNIT(*)
SI_UNIT(.KILO.,.GRAM.)
);
#6898=DERIVED_UNIT((#6861,#6862));
#6899=DERIVED_UNIT((#6863,#6864));
#6900=DERIVED_UNIT((#6865,#6866));
#6901=DERIVED_UNIT((#6867,#6868));
#6902=DERIVED_UNIT((#6869,#6870));
#6903=DERIVED_UNIT((#6871,#6872));
#6904=DERIVED_UNIT((#6873,#6874));
#6905=DERIVED_UNIT((#6875,#6876));
#6906=DERIVED_UNIT((#6877,#6878));
#6907=DERIVED_UNIT((#6879,#6880));
#6908=DERIVED_UNIT((#6881,#6882));
#6909=DERIVED_UNIT((#6883,#6884));
#6910=DERIVED_UNIT((#6885,#6886));
#6911=DERIVED_UNIT((#6887,#6888));
#6912=DERIVED_UNIT((#6889,#6890));
#6913=DERIVED_UNIT((#6891,#6892));
#6914=DERIVED_UNIT((#6893,#6894));
#6915=DERIVED_UNIT((#6895,#6896));
#6916=MEASURE_REPRESENTATION_ITEM('density measure',
POSITIVE_RATIO_MEASURE(7850.),#6898);
#6917=MEASURE_REPRESENTATION_ITEM('density measure',
POSITIVE_RATIO_MEASURE(7850.),#6899);
#6918=MEASURE_REPRESENTATION_ITEM('density measure',
POSITIVE_RATIO_MEASURE(7850.),#6900);
#6919=MEASURE_REPRESENTATION_ITEM('density measure',
POSITIVE_RATIO_MEASURE(7850.),#6901);
#6920=MEASURE_REPRESENTATION_ITEM('density measure',
POSITIVE_RATIO_MEASURE(7850.),#6902);
#6921=MEASURE_REPRESENTATION_ITEM('density measure',
POSITIVE_RATIO_MEASURE(7850.),#6903);
#6922=MEASURE_REPRESENTATION_ITEM('density measure',
POSITIVE_RATIO_MEASURE(7850.),#6904);
#6923=MEASURE_REPRESENTATION_ITEM('density measure',
POSITIVE_RATIO_MEASURE(7850.),#6905);
#6924=MEASURE_REPRESENTATION_ITEM('density measure',
POSITIVE_RATIO_MEASURE(7850.),#6906);
#6925=MEASURE_REPRESENTATION_ITEM('density measure',
POSITIVE_RATIO_MEASURE(7850.),#6907);
#6926=MEASURE_REPRESENTATION_ITEM('density measure',
POSITIVE_RATIO_MEASURE(7850.),#6908);
#6927=MEASURE_REPRESENTATION_ITEM('density measure',
POSITIVE_RATIO_MEASURE(7850.),#6909);
#6928=MEASURE_REPRESENTATION_ITEM('density measure',
POSITIVE_RATIO_MEASURE(7850.),#6910);
#6929=MEASURE_REPRESENTATION_ITEM('density measure',
POSITIVE_RATIO_MEASURE(7850.),#6911);
#6930=MEASURE_REPRESENTATION_ITEM('density measure',
POSITIVE_RATIO_MEASURE(7850.),#6912);
#6931=MEASURE_REPRESENTATION_ITEM('density measure',
POSITIVE_RATIO_MEASURE(7850.),#6913);
#6932=MEASURE_REPRESENTATION_ITEM('density measure',
POSITIVE_RATIO_MEASURE(7850.),#6914);
#6933=MEASURE_REPRESENTATION_ITEM('density measure',
POSITIVE_RATIO_MEASURE(7850.),#6915);
#6934=PROPERTY_DEFINITION_REPRESENTATION(#7024,#6970);
#6935=PROPERTY_DEFINITION_REPRESENTATION(#7025,#6971);
#6936=PROPERTY_DEFINITION_REPRESENTATION(#7026,#6972);
#6937=PROPERTY_DEFINITION_REPRESENTATION(#7027,#6973);
#6938=PROPERTY_DEFINITION_REPRESENTATION(#7028,#6974);
#6939=PROPERTY_DEFINITION_REPRESENTATION(#7029,#6975);
#6940=PROPERTY_DEFINITION_REPRESENTATION(#7030,#6976);
#6941=PROPERTY_DEFINITION_REPRESENTATION(#7031,#6977);
#6942=PROPERTY_DEFINITION_REPRESENTATION(#7032,#6978);
#6943=PROPERTY_DEFINITION_REPRESENTATION(#7033,#6979);
#6944=PROPERTY_DEFINITION_REPRESENTATION(#7034,#6980);
#6945=PROPERTY_DEFINITION_REPRESENTATION(#7035,#6981);
#6946=PROPERTY_DEFINITION_REPRESENTATION(#7036,#6982);
#6947=PROPERTY_DEFINITION_REPRESENTATION(#7037,#6983);
#6948=PROPERTY_DEFINITION_REPRESENTATION(#7038,#6984);
#6949=PROPERTY_DEFINITION_REPRESENTATION(#7039,#6985);
#6950=PROPERTY_DEFINITION_REPRESENTATION(#7040,#6986);
#6951=PROPERTY_DEFINITION_REPRESENTATION(#7041,#6987);
#6952=PROPERTY_DEFINITION_REPRESENTATION(#7042,#6988);
#6953=PROPERTY_DEFINITION_REPRESENTATION(#7043,#6989);
#6954=PROPERTY_DEFINITION_REPRESENTATION(#7044,#6990);
#6955=PROPERTY_DEFINITION_REPRESENTATION(#7045,#6991);
#6956=PROPERTY_DEFINITION_REPRESENTATION(#7046,#6992);
#6957=PROPERTY_DEFINITION_REPRESENTATION(#7047,#6993);
#6958=PROPERTY_DEFINITION_REPRESENTATION(#7048,#6994);
#6959=PROPERTY_DEFINITION_REPRESENTATION(#7049,#6995);
#6960=PROPERTY_DEFINITION_REPRESENTATION(#7050,#6996);
#6961=PROPERTY_DEFINITION_REPRESENTATION(#7051,#6997);
#6962=PROPERTY_DEFINITION_REPRESENTATION(#7052,#6998);
#6963=PROPERTY_DEFINITION_REPRESENTATION(#7053,#6999);
#6964=PROPERTY_DEFINITION_REPRESENTATION(#7054,#7000);
#6965=PROPERTY_DEFINITION_REPRESENTATION(#7055,#7001);
#6966=PROPERTY_DEFINITION_REPRESENTATION(#7056,#7002);
#6967=PROPERTY_DEFINITION_REPRESENTATION(#7057,#7003);
#6968=PROPERTY_DEFINITION_REPRESENTATION(#7058,#7004);
#6969=PROPERTY_DEFINITION_REPRESENTATION(#7059,#7005);
#6970=REPRESENTATION('material name',(#7006),#13175);
#6971=REPRESENTATION('density',(#6916),#13175);
#6972=REPRESENTATION('material name',(#7007),#13177);
#6973=REPRESENTATION('density',(#6917),#13177);
#6974=REPRESENTATION('material name',(#7008),#13178);
#6975=REPRESENTATION('density',(#6918),#13178);
#6976=REPRESENTATION('material name',(#7009),#13179);
#6977=REPRESENTATION('density',(#6919),#13179);
#6978=REPRESENTATION('material name',(#7010),#13181);
#6979=REPRESENTATION('density',(#6920),#13181);
#6980=REPRESENTATION('material name',(#7011),#13182);
#6981=REPRESENTATION('density',(#6921),#13182);
#6982=REPRESENTATION('material name',(#7012),#13184);
#6983=REPRESENTATION('density',(#6922),#13184);
#6984=REPRESENTATION('material name',(#7013),#13185);
#6985=REPRESENTATION('density',(#6923),#13185);
#6986=REPRESENTATION('material name',(#7014),#13187);
#6987=REPRESENTATION('density',(#6924),#13187);
#6988=REPRESENTATION('material name',(#7015),#13188);
#6989=REPRESENTATION('density',(#6925),#13188);
#6990=REPRESENTATION('material name',(#7016),#13189);
#6991=REPRESENTATION('density',(#6926),#13189);
#6992=REPRESENTATION('material name',(#7017),#13190);
#6993=REPRESENTATION('density',(#6927),#13190);
#6994=REPRESENTATION('material name',(#7018),#13192);
#6995=REPRESENTATION('density',(#6928),#13192);
#6996=REPRESENTATION('material name',(#7019),#13193);
#6997=REPRESENTATION('density',(#6929),#13193);
#6998=REPRESENTATION('material name',(#7020),#13194);
#6999=REPRESENTATION('density',(#6930),#13194);
#7000=REPRESENTATION('material name',(#7021),#13195);
#7001=REPRESENTATION('density',(#6931),#13195);
#7002=REPRESENTATION('material name',(#7022),#13197);
#7003=REPRESENTATION('density',(#6932),#13197);
#7004=REPRESENTATION('material name',(#7023),#13198);
#7005=REPRESENTATION('density',(#6933),#13198);
#7006=DESCRIPTIVE_REPRESENTATION_ITEM('Steel','Steel');
#7007=DESCRIPTIVE_REPRESENTATION_ITEM('Steel','Steel');
#7008=DESCRIPTIVE_REPRESENTATION_ITEM('Steel','Steel');
#7009=DESCRIPTIVE_REPRESENTATION_ITEM('Steel','Steel');
#7010=DESCRIPTIVE_REPRESENTATION_ITEM('Steel','Steel');
#7011=DESCRIPTIVE_REPRESENTATION_ITEM('Steel','Steel');
#7012=DESCRIPTIVE_REPRESENTATION_ITEM('Steel','Steel');
#7013=DESCRIPTIVE_REPRESENTATION_ITEM('Steel','Steel');
#7014=DESCRIPTIVE_REPRESENTATION_ITEM('Steel','Steel');
#7015=DESCRIPTIVE_REPRESENTATION_ITEM('Steel','Steel');
#7016=DESCRIPTIVE_REPRESENTATION_ITEM('Steel','Steel');
#7017=DESCRIPTIVE_REPRESENTATION_ITEM('Steel','Steel');
#7018=DESCRIPTIVE_REPRESENTATION_ITEM('Steel','Steel');
#7019=DESCRIPTIVE_REPRESENTATION_ITEM('Steel','Steel');
#7020=DESCRIPTIVE_REPRESENTATION_ITEM('Steel','Steel');
#7021=DESCRIPTIVE_REPRESENTATION_ITEM('Steel','Steel');
#7022=DESCRIPTIVE_REPRESENTATION_ITEM('Steel','Steel');
#7023=DESCRIPTIVE_REPRESENTATION_ITEM('Steel','Steel');
#7024=PROPERTY_DEFINITION('material property','material name',#13305);
#7025=PROPERTY_DEFINITION('material property','density of part',#13305);
#7026=PROPERTY_DEFINITION('material property','material name',#13307);
#7027=PROPERTY_DEFINITION('material property','density of part',#13307);
#7028=PROPERTY_DEFINITION('material property','material name',#13308);
#7029=PROPERTY_DEFINITION('material property','density of part',#13308);
#7030=PROPERTY_DEFINITION('material property','material name',#13309);
#7031=PROPERTY_DEFINITION('material property','density of part',#13309);
#7032=PROPERTY_DEFINITION('material property','material name',#13311);
#7033=PROPERTY_DEFINITION('material property','density of part',#13311);
#7034=PROPERTY_DEFINITION('material property','material name',#13312);
#7035=PROPERTY_DEFINITION('material property','density of part',#13312);
#7036=PROPERTY_DEFINITION('material property','material name',#13314);
#7037=PROPERTY_DEFINITION('material property','density of part',#13314);
#7038=PROPERTY_DEFINITION('material property','material name',#13315);
#7039=PROPERTY_DEFINITION('material property','density of part',#13315);
#7040=PROPERTY_DEFINITION('material property','material name',#13317);
#7041=PROPERTY_DEFINITION('material property','density of part',#13317);
#7042=PROPERTY_DEFINITION('material property','material name',#13318);
#7043=PROPERTY_DEFINITION('material property','density of part',#13318);
#7044=PROPERTY_DEFINITION('material property','material name',#13319);
#7045=PROPERTY_DEFINITION('material property','density of part',#13319);
#7046=PROPERTY_DEFINITION('material property','material name',#13320);
#7047=PROPERTY_DEFINITION('material property','density of part',#13320);
#7048=PROPERTY_DEFINITION('material property','material name',#13322);
#7049=PROPERTY_DEFINITION('material property','density of part',#13322);
#7050=PROPERTY_DEFINITION('material property','material name',#13323);
#7051=PROPERTY_DEFINITION('material property','density of part',#13323);
#7052=PROPERTY_DEFINITION('material property','material name',#13324);
#7053=PROPERTY_DEFINITION('material property','density of part',#13324);
#7054=PROPERTY_DEFINITION('material property','material name',#13325);
#7055=PROPERTY_DEFINITION('material property','density of part',#13325);
#7056=PROPERTY_DEFINITION('material property','material name',#13327);
#7057=PROPERTY_DEFINITION('material property','density of part',#13327);
#7058=PROPERTY_DEFINITION('material property','material name',#13328);
#7059=PROPERTY_DEFINITION('material property','density of part',#13328);
#7060=AXIS2_PLACEMENT_3D('',#9885,#7829,#7830);
#7061=AXIS2_PLACEMENT_3D('',#9886,#7831,#7832);
#7062=AXIS2_PLACEMENT_3D('',#9887,#7833,#7834);
#7063=AXIS2_PLACEMENT_3D('',#9890,#7835,#7836);
#7064=AXIS2_PLACEMENT_3D('',#9892,#7837,#7838);
#7065=AXIS2_PLACEMENT_3D('',#9894,#7839,#7840);
#7066=AXIS2_PLACEMENT_3D('',#9895,#7841,#7842);
#7067=AXIS2_PLACEMENT_3D('',#9896,#7843,#7844);
#7068=AXIS2_PLACEMENT_3D('',#9899,#7845,#7846);
#7069=AXIS2_PLACEMENT_3D('',#9901,#7847,#7848);
#7070=AXIS2_PLACEMENT_3D('',#9903,#7849,#7850);
#7071=AXIS2_PLACEMENT_3D('',#9904,#7851,#7852);
#7072=AXIS2_PLACEMENT_3D('',#9905,#7853,#7854);
#7073=AXIS2_PLACEMENT_3D('',#9908,#7855,#7856);
#7074=AXIS2_PLACEMENT_3D('',#9910,#7857,#7858);
#7075=AXIS2_PLACEMENT_3D('',#9911,#7859,#7860);
#7076=AXIS2_PLACEMENT_3D('',#9912,#7861,#7862);
#7077=AXIS2_PLACEMENT_3D('',#9914,#7863,#7864);
#7078=AXIS2_PLACEMENT_3D('',#9917,#7866,#7867);
#7079=AXIS2_PLACEMENT_3D('',#9918,#7868,#7869);
#7080=AXIS2_PLACEMENT_3D('',#9920,#7870,#7871);
#7081=AXIS2_PLACEMENT_3D('',#9923,#7873,#7874);
#7082=AXIS2_PLACEMENT_3D('',#9924,#7875,#7876);
#7083=AXIS2_PLACEMENT_3D('',#9926,#7877,#7878);
#7084=AXIS2_PLACEMENT_3D('',#9929,#7880,#7881);
#7085=AXIS2_PLACEMENT_3D('',#9931,#7883,#7884);
#7086=AXIS2_PLACEMENT_3D('',#9939,#7888,#7889);
#7087=AXIS2_PLACEMENT_3D('',#9940,#7890,#7891);
#7088=AXIS2_PLACEMENT_3D('',#9945,#7893,#7894);
#7089=AXIS2_PLACEMENT_3D('',#9949,#7896,#7897);
#7090=AXIS2_PLACEMENT_3D('',#9952,#7899,#7900);
#7091=AXIS2_PLACEMENT_3D('',#9953,#7901,#7902);
#7092=AXIS2_PLACEMENT_3D('',#9954,#7903,#7904);
#7093=AXIS2_PLACEMENT_3D('',#9959,#7907,#7908);
#7094=AXIS2_PLACEMENT_3D('',#9960,#7909,#7910);
#7095=AXIS2_PLACEMENT_3D('',#9964,#7912,#7913);
#7096=AXIS2_PLACEMENT_3D('',#9965,#7914,#7915);
#7097=AXIS2_PLACEMENT_3D('',#9967,#7916,#7917);
#7098=AXIS2_PLACEMENT_3D('',#9970,#7919,#7920);
#7099=AXIS2_PLACEMENT_3D('',#9971,#7921,#7922);
#7100=AXIS2_PLACEMENT_3D('',#9974,#7923,#7924);
#7101=AXIS2_PLACEMENT_3D('',#9977,#7926,#7927);
#7102=AXIS2_PLACEMENT_3D('',#9983,#7930,#7931);
#7103=AXIS2_PLACEMENT_3D('',#9986,#7933,#7934);
#7104=AXIS2_PLACEMENT_3D('',#9987,#7935,#7936);
#7105=AXIS2_PLACEMENT_3D('',#9996,#7941,#7942);
#7106=AXIS2_PLACEMENT_3D('',#9998,#7944,#7945);
#7107=AXIS2_PLACEMENT_3D('',#10007,#7950,#7951);
#7108=AXIS2_PLACEMENT_3D('',#10016,#7956,#7957);
#7109=AXIS2_PLACEMENT_3D('',#10025,#7962,#7963);
#7110=AXIS2_PLACEMENT_3D('',#10033,#7968,#7969);
#7111=AXIS2_PLACEMENT_3D('',#10036,#7970,#7971);
#7112=AXIS2_PLACEMENT_3D('',#10037,#7972,#7973);
#7113=AXIS2_PLACEMENT_3D('',#10039,#7974,#7975);
#7114=AXIS2_PLACEMENT_3D('',#10047,#7980,#7981);
#7115=AXIS2_PLACEMENT_3D('',#10049,#7982,#7983);
#7116=AXIS2_PLACEMENT_3D('',#10051,#7984,#7985);
#7117=AXIS2_PLACEMENT_3D('',#10052,#7986,#7987);
#7118=AXIS2_PLACEMENT_3D('',#10060,#7992,#7993);
#7119=AXIS2_PLACEMENT_3D('',#10064,#7995,#7996);
#7120=AXIS2_PLACEMENT_3D('',#10069,#8000,#8001);
#7121=AXIS2_PLACEMENT_3D('',#10073,#8003,#8004);
#7122=AXIS2_PLACEMENT_3D('',#10078,#8008,#8009);
#7123=AXIS2_PLACEMENT_3D('',#10080,#8011,#8012);
#7124=AXIS2_PLACEMENT_3D('',#10082,#8014,#8015);
#7125=AXIS2_PLACEMENT_3D('',#10083,#8016,#8017);
#7126=AXIS2_PLACEMENT_3D('',#10085,#8019,#8020);
#7127=AXIS2_PLACEMENT_3D('',#10086,#8021,#8022);
#7128=AXIS2_PLACEMENT_3D('',#10087,#8023,#8024);
#7129=AXIS2_PLACEMENT_3D('',#10088,#8025,#8026);
#7130=AXIS2_PLACEMENT_3D('',#10089,#8027,#8028);
#7131=AXIS2_PLACEMENT_3D('',#10090,#8029,#8030);
#7132=AXIS2_PLACEMENT_3D('',#10091,#8031,#8032);
#7133=AXIS2_PLACEMENT_3D('',#10092,#8033,#8034);
#7134=AXIS2_PLACEMENT_3D('',#10093,#8035,#8036);
#7135=AXIS2_PLACEMENT_3D('',#10094,#8037,#8038);
#7136=AXIS2_PLACEMENT_3D('',#10095,#8039,#8040);
#7137=AXIS2_PLACEMENT_3D('',#10096,#8041,#8042);
#7138=AXIS2_PLACEMENT_3D('',#10097,#8043,#8044);
#7139=AXIS2_PLACEMENT_3D('',#10098,#8045,#8046);
#7140=AXIS2_PLACEMENT_3D('',#10099,#8047,#8048);
#7141=AXIS2_PLACEMENT_3D('',#10100,#8049,#8050);
#7142=AXIS2_PLACEMENT_3D('',#10101,#8051,#8052);
#7143=AXIS2_PLACEMENT_3D('',#10102,#8053,#8054);
#7144=AXIS2_PLACEMENT_3D('',#10103,#8055,#8056);
#7145=AXIS2_PLACEMENT_3D('',#10104,#8057,#8058);
#7146=AXIS2_PLACEMENT_3D('',#10105,#8059,#8060);
#7147=AXIS2_PLACEMENT_3D('',#10106,#8061,#8062);
#7148=AXIS2_PLACEMENT_3D('',#10107,#8063,#8064);
#7149=AXIS2_PLACEMENT_3D('',#10108,#8065,#8066);
#7150=AXIS2_PLACEMENT_3D('',#10109,#8067,#8068);
#7151=AXIS2_PLACEMENT_3D('',#10110,#8069,#8070);
#7152=AXIS2_PLACEMENT_3D('',#10111,#8071,#8072);
#7153=AXIS2_PLACEMENT_3D('',#10112,#8073,#8074);
#7154=AXIS2_PLACEMENT_3D('',#10113,#8075,#8076);
#7155=AXIS2_PLACEMENT_3D('',#10114,#8077,#8078);
#7156=AXIS2_PLACEMENT_3D('',#10115,#8079,#8080);
#7157=AXIS2_PLACEMENT_3D('',#10116,#8081,#8082);
#7158=AXIS2_PLACEMENT_3D('',#10117,#8083,#8084);
#7159=AXIS2_PLACEMENT_3D('',#10118,#8085,#8086);
#7160=AXIS2_PLACEMENT_3D('',#10119,#8087,#8088);
#7161=AXIS2_PLACEMENT_3D('',#10120,#8089,#8090);
#7162=AXIS2_PLACEMENT_3D('',#10121,#8091,#8092);
#7163=AXIS2_PLACEMENT_3D('',#10122,#8093,#8094);
#7164=AXIS2_PLACEMENT_3D('',#10123,#8095,#8096);
#7165=AXIS2_PLACEMENT_3D('',#10124,#8097,#8098);
#7166=AXIS2_PLACEMENT_3D('',#10125,#8099,#8100);
#7167=AXIS2_PLACEMENT_3D('',#10126,#8101,#8102);
#7168=AXIS2_PLACEMENT_3D('',#10127,#8103,#8104);
#7169=AXIS2_PLACEMENT_3D('',#10128,#8105,#8106);
#7170=AXIS2_PLACEMENT_3D('',#10129,#8107,#8108);
#7171=AXIS2_PLACEMENT_3D('',#10130,#8109,#8110);
#7172=AXIS2_PLACEMENT_3D('',#10131,#8111,#8112);
#7173=AXIS2_PLACEMENT_3D('',#10132,#8113,#8114);
#7174=AXIS2_PLACEMENT_3D('',#10133,#8115,#8116);
#7175=AXIS2_PLACEMENT_3D('',#10134,#8117,#8118);
#7176=AXIS2_PLACEMENT_3D('',#10135,#8119,#8120);
#7177=AXIS2_PLACEMENT_3D('',#10136,#8121,#8122);
#7178=AXIS2_PLACEMENT_3D('',#10137,#8123,#8124);
#7179=AXIS2_PLACEMENT_3D('',#10138,#8125,#8126);
#7180=AXIS2_PLACEMENT_3D('',#10139,#8127,#8128);
#7181=AXIS2_PLACEMENT_3D('',#10140,#8129,#8130);
#7182=AXIS2_PLACEMENT_3D('',#10141,#8131,#8132);
#7183=AXIS2_PLACEMENT_3D('',#10142,#8133,#8134);
#7184=AXIS2_PLACEMENT_3D('',#10143,#8135,#8136);
#7185=AXIS2_PLACEMENT_3D('',#10144,#8137,#8138);
#7186=AXIS2_PLACEMENT_3D('',#10145,#8139,#8140);
#7187=AXIS2_PLACEMENT_3D('',#10146,#8141,#8142);
#7188=AXIS2_PLACEMENT_3D('',#10149,#8145,#8146);
#7189=AXIS2_PLACEMENT_3D('',#10151,#8148,#8149);
#7190=AXIS2_PLACEMENT_3D('',#10153,#8151,#8152);
#7191=AXIS2_PLACEMENT_3D('',#10154,#8153,#8154);
#7192=AXIS2_PLACEMENT_3D('',#10155,#8155,#8156);
#7193=AXIS2_PLACEMENT_3D('',#10156,#8157,#8158);
#7194=AXIS2_PLACEMENT_3D('',#10157,#8159,#8160);
#7195=AXIS2_PLACEMENT_3D('',#10179,#8161,#8162);
#7196=AXIS2_PLACEMENT_3D('',#10183,#8164,#8165);
#7197=AXIS2_PLACEMENT_3D('',#10187,#8167,#8168);
#7198=AXIS2_PLACEMENT_3D('',#10191,#8170,#8171);
#7199=AXIS2_PLACEMENT_3D('',#10194,#8173,#8174);
#7200=AXIS2_PLACEMENT_3D('',#10195,#8175,#8176);
#7201=AXIS2_PLACEMENT_3D('',#10197,#8177,#8178);
#7202=AXIS2_PLACEMENT_3D('',#10200,#8180,#8181);
#7203=AXIS2_PLACEMENT_3D('',#10201,#8182,#8183);
#7204=AXIS2_PLACEMENT_3D('',#10203,#8184,#8185);
#7205=AXIS2_PLACEMENT_3D('',#10206,#8187,#8188);
#7206=AXIS2_PLACEMENT_3D('',#10207,#8189,#8190);
#7207=AXIS2_PLACEMENT_3D('',#10209,#8191,#8192);
#7208=AXIS2_PLACEMENT_3D('',#10212,#8194,#8195);
#7209=AXIS2_PLACEMENT_3D('',#10213,#8196,#8197);
#7210=AXIS2_PLACEMENT_3D('',#10215,#8198,#8199);
#7211=AXIS2_PLACEMENT_3D('',#10218,#8201,#8202);
#7212=AXIS2_PLACEMENT_3D('',#10219,#8203,#8204);
#7213=AXIS2_PLACEMENT_3D('',#10221,#8205,#8206);
#7214=AXIS2_PLACEMENT_3D('',#10262,#8208,#8209);
#7215=AXIS2_PLACEMENT_3D('',#10285,#8211,#8212);
#7216=AXIS2_PLACEMENT_3D('',#10305,#8213,#8214);
#7217=AXIS2_PLACEMENT_3D('',#10308,#8215,#8216);
#7218=AXIS2_PLACEMENT_3D('',#10342,#8217,#8218);
#7219=AXIS2_PLACEMENT_3D('',#10399,#8220,#8221);
#7220=AXIS2_PLACEMENT_3D('',#10431,#8222,#8223);
#7221=AXIS2_PLACEMENT_3D('',#10435,#8226,#8227);
#7222=AXIS2_PLACEMENT_3D('',#10438,#8229,#8230);
#7223=AXIS2_PLACEMENT_3D('',#10439,#8231,#8232);
#7224=AXIS2_PLACEMENT_3D('',#10444,#8235,#8236);
#7225=AXIS2_PLACEMENT_3D('',#10445,#8237,#8238);
#7226=AXIS2_PLACEMENT_3D('',#10454,#8243,#8244);
#7227=AXIS2_PLACEMENT_3D('',#10455,#8245,#8246);
#7228=AXIS2_PLACEMENT_3D('',#10466,#8247,#8248);
#7229=AXIS2_PLACEMENT_3D('',#10470,#8250,#8251);
#7230=AXIS2_PLACEMENT_3D('',#10471,#8252,#8253);
#7231=AXIS2_PLACEMENT_3D('',#10472,#8254,#8255);
#7232=AXIS2_PLACEMENT_3D('',#10477,#8257,#8258);
#7233=AXIS2_PLACEMENT_3D('',#10480,#8260,#8261);
#7234=AXIS2_PLACEMENT_3D('',#10481,#8262,#8263);
#7235=AXIS2_PLACEMENT_3D('',#10487,#8267,#8268);
#7236=AXIS2_PLACEMENT_3D('',#10489,#8270,#8271);
#7237=AXIS2_PLACEMENT_3D('',#10491,#8273,#8274);
#7238=AXIS2_PLACEMENT_3D('',#10492,#8275,#8276);
#7239=AXIS2_PLACEMENT_3D('',#10498,#8280,#8281);
#7240=AXIS2_PLACEMENT_3D('',#10503,#8283,#8284);
#7241=AXIS2_PLACEMENT_3D('',#10509,#8288,#8289);
#7242=AXIS2_PLACEMENT_3D('',#10510,#8290,#8291);
#7243=AXIS2_PLACEMENT_3D('',#10514,#8294,#8295);
#7244=AXIS2_PLACEMENT_3D('',#10517,#8297,#8298);
#7245=AXIS2_PLACEMENT_3D('',#10519,#8299,#8300);
#7246=AXIS2_PLACEMENT_3D('',#10521,#8302,#8303);
#7247=AXIS2_PLACEMENT_3D('',#10529,#8309,#8310);
#7248=AXIS2_PLACEMENT_3D('',#10536,#8315,#8316);
#7249=AXIS2_PLACEMENT_3D('',#10542,#8320,#8321);
#7250=AXIS2_PLACEMENT_3D('',#10544,#8323,#8324);
#7251=AXIS2_PLACEMENT_3D('',#10545,#8325,#8326);
#7252=AXIS2_PLACEMENT_3D('',#10546,#8327,#8328);
#7253=AXIS2_PLACEMENT_3D('',#10547,#8329,#8330);
#7254=AXIS2_PLACEMENT_3D('',#10548,#8331,#8332);
#7255=AXIS2_PLACEMENT_3D('',#10549,#8333,#8334);
#7256=AXIS2_PLACEMENT_3D('',#10550,#8335,#8336);
#7257=AXIS2_PLACEMENT_3D('',#10551,#8337,#8338);
#7258=AXIS2_PLACEMENT_3D('',#10552,#8339,#8340);
#7259=AXIS2_PLACEMENT_3D('',#10553,#8341,#8342);
#7260=AXIS2_PLACEMENT_3D('',#10554,#8343,#8344);
#7261=AXIS2_PLACEMENT_3D('',#10555,#8345,#8346);
#7262=AXIS2_PLACEMENT_3D('',#10556,#8347,#8348);
#7263=AXIS2_PLACEMENT_3D('',#10557,#8349,#8350);
#7264=AXIS2_PLACEMENT_3D('',#10566,#8355,#8356);
#7265=AXIS2_PLACEMENT_3D('',#10569,#8358,#8359);
#7266=AXIS2_PLACEMENT_3D('',#10571,#8360,#8361);
#7267=AXIS2_PLACEMENT_3D('',#10573,#8363,#8364);
#7268=AXIS2_PLACEMENT_3D('',#10577,#8367,#8368);
#7269=AXIS2_PLACEMENT_3D('',#10578,#8369,#8370);
#7270=AXIS2_PLACEMENT_3D('',#10581,#8372,#8373);
#7271=AXIS2_PLACEMENT_3D('',#10582,#8374,#8375);
#7272=AXIS2_PLACEMENT_3D('',#10584,#8377,#8378);
#7273=AXIS2_PLACEMENT_3D('',#10585,#8379,#8380);
#7274=AXIS2_PLACEMENT_3D('',#10586,#8381,#8382);
#7275=AXIS2_PLACEMENT_3D('',#10587,#8383,#8384);
#7276=AXIS2_PLACEMENT_3D('',#10589,#8385,#8386);
#7277=AXIS2_PLACEMENT_3D('',#10592,#8388,#8389);
#7278=AXIS2_PLACEMENT_3D('',#10593,#8390,#8391);
#7279=AXIS2_PLACEMENT_3D('',#10595,#8392,#8393);
#7280=AXIS2_PLACEMENT_3D('',#10598,#8395,#8396);
#7281=AXIS2_PLACEMENT_3D('',#10599,#8397,#8398);
#7282=AXIS2_PLACEMENT_3D('',#10601,#8399,#8400);
#7283=AXIS2_PLACEMENT_3D('',#10604,#8402,#8403);
#7284=AXIS2_PLACEMENT_3D('',#10605,#8404,#8405);
#7285=AXIS2_PLACEMENT_3D('',#10607,#8406,#8407);
#7286=AXIS2_PLACEMENT_3D('',#10610,#8409,#8410);
#7287=AXIS2_PLACEMENT_3D('',#10611,#8411,#8412);
#7288=AXIS2_PLACEMENT_3D('',#10613,#8413,#8414);
#7289=AXIS2_PLACEMENT_3D('',#10654,#8416,#8417);
#7290=AXIS2_PLACEMENT_3D('',#10677,#8419,#8420);
#7291=AXIS2_PLACEMENT_3D('',#10697,#8421,#8422);
#7292=AXIS2_PLACEMENT_3D('',#10700,#8423,#8424);
#7293=AXIS2_PLACEMENT_3D('',#10748,#8425,#8426);
#7294=AXIS2_PLACEMENT_3D('',#10797,#8428,#8429);
#7295=AXIS2_PLACEMENT_3D('',#10843,#8430,#8431);
#7296=AXIS2_PLACEMENT_3D('',#10846,#8432,#8433);
#7297=AXIS2_PLACEMENT_3D('',#10861,#8436,#8437);
#7298=AXIS2_PLACEMENT_3D('',#10863,#8439,#8440);
#7299=AXIS2_PLACEMENT_3D('',#10872,#8445,#8446);
#7300=AXIS2_PLACEMENT_3D('',#10873,#8447,#8448);
#7301=AXIS2_PLACEMENT_3D('',#10874,#8449,#8450);
#7302=AXIS2_PLACEMENT_3D('',#10879,#8452,#8453);
#7303=AXIS2_PLACEMENT_3D('',#10882,#8455,#8456);
#7304=AXIS2_PLACEMENT_3D('',#10883,#8457,#8458);
#7305=AXIS2_PLACEMENT_3D('',#10886,#8459,#8460);
#7306=AXIS2_PLACEMENT_3D('',#10892,#8464,#8465);
#7307=AXIS2_PLACEMENT_3D('',#10894,#8466,#8467);
#7308=AXIS2_PLACEMENT_3D('',#10895,#8468,#8469);
#7309=AXIS2_PLACEMENT_3D('',#10910,#8471,#8472);
#7310=AXIS2_PLACEMENT_3D('',#10912,#8473,#8474);
#7311=AXIS2_PLACEMENT_3D('',#10913,#8475,#8476);
#7312=AXIS2_PLACEMENT_3D('',#10928,#8478,#8479);
#7313=AXIS2_PLACEMENT_3D('',#10929,#8480,#8481);
#7314=AXIS2_PLACEMENT_3D('',#10935,#8485,#8486);
#7315=AXIS2_PLACEMENT_3D('',#10940,#8488,#8489);
#7316=AXIS2_PLACEMENT_3D('',#10946,#8493,#8494);
#7317=AXIS2_PLACEMENT_3D('',#10947,#8495,#8496);
#7318=AXIS2_PLACEMENT_3D('',#10951,#8499,#8500);
#7319=AXIS2_PLACEMENT_3D('',#10954,#8502,#8503);
#7320=AXIS2_PLACEMENT_3D('',#10956,#8504,#8505);
#7321=AXIS2_PLACEMENT_3D('',#10958,#8507,#8508);
#7322=AXIS2_PLACEMENT_3D('',#10968,#8514,#8515);
#7323=AXIS2_PLACEMENT_3D('',#10978,#8521,#8522);
#7324=AXIS2_PLACEMENT_3D('',#10984,#8526,#8527);
#7325=AXIS2_PLACEMENT_3D('',#10993,#8532,#8533);
#7326=AXIS2_PLACEMENT_3D('',#10994,#8534,#8535);
#7327=AXIS2_PLACEMENT_3D('',#10995,#8536,#8537);
#7328=AXIS2_PLACEMENT_3D('',#10996,#8538,#8539);
#7329=AXIS2_PLACEMENT_3D('',#10997,#8540,#8541);
#7330=AXIS2_PLACEMENT_3D('',#10998,#8542,#8543);
#7331=AXIS2_PLACEMENT_3D('',#10999,#8544,#8545);
#7332=AXIS2_PLACEMENT_3D('',#11000,#8546,#8547);
#7333=AXIS2_PLACEMENT_3D('',#11001,#8548,#8549);
#7334=AXIS2_PLACEMENT_3D('',#11002,#8550,#8551);
#7335=AXIS2_PLACEMENT_3D('',#11003,#8552,#8553);
#7336=AXIS2_PLACEMENT_3D('',#11004,#8554,#8555);
#7337=AXIS2_PLACEMENT_3D('',#11005,#8556,#8557);
#7338=AXIS2_PLACEMENT_3D('',#11006,#8558,#8559);
#7339=AXIS2_PLACEMENT_3D('',#11007,#8560,#8561);
#7340=AXIS2_PLACEMENT_3D('',#11008,#8562,#8563);
#7341=AXIS2_PLACEMENT_3D('',#11009,#8564,#8565);
#7342=AXIS2_PLACEMENT_3D('',#11010,#8566,#8567);
#7343=AXIS2_PLACEMENT_3D('',#11011,#8568,#8569);
#7344=AXIS2_PLACEMENT_3D('',#11020,#8574,#8575);
#7345=AXIS2_PLACEMENT_3D('',#11023,#8577,#8578);
#7346=AXIS2_PLACEMENT_3D('',#11025,#8579,#8580);
#7347=AXIS2_PLACEMENT_3D('',#11027,#8582,#8583);
#7348=AXIS2_PLACEMENT_3D('',#11031,#8586,#8587);
#7349=AXIS2_PLACEMENT_3D('',#11032,#8588,#8589);
#7350=AXIS2_PLACEMENT_3D('',#11035,#8591,#8592);
#7351=AXIS2_PLACEMENT_3D('',#11036,#8593,#8594);
#7352=AXIS2_PLACEMENT_3D('',#11038,#8596,#8597);
#7353=AXIS2_PLACEMENT_3D('',#11039,#8598,#8599);
#7354=AXIS2_PLACEMENT_3D('',#11040,#8600,#8601);
#7355=AXIS2_PLACEMENT_3D('',#11042,#8603,#8604);
#7356=AXIS2_PLACEMENT_3D('',#11044,#8606,#8607);
#7357=AXIS2_PLACEMENT_3D('',#11045,#8608,#8609);
#7358=AXIS2_PLACEMENT_3D('',#11046,#8610,#8611);
#7359=AXIS2_PLACEMENT_3D('',#11047,#8612,#8613);
#7360=AXIS2_PLACEMENT_3D('',#11048,#8614,#8615);
#7361=AXIS2_PLACEMENT_3D('',#11050,#8616,#8617);
#7362=AXIS2_PLACEMENT_3D('',#11053,#8619,#8620);
#7363=AXIS2_PLACEMENT_3D('',#11054,#8621,#8622);
#7364=AXIS2_PLACEMENT_3D('',#11056,#8623,#8624);
#7365=AXIS2_PLACEMENT_3D('',#11059,#8626,#8627);
#7366=AXIS2_PLACEMENT_3D('',#11060,#8628,#8629);
#7367=AXIS2_PLACEMENT_3D('',#11062,#8630,#8631);
#7368=AXIS2_PLACEMENT_3D('',#11065,#8633,#8634);
#7369=AXIS2_PLACEMENT_3D('',#11066,#8635,#8636);
#7370=AXIS2_PLACEMENT_3D('',#11068,#8637,#8638);
#7371=AXIS2_PLACEMENT_3D('',#11071,#8640,#8641);
#7372=AXIS2_PLACEMENT_3D('',#11072,#8642,#8643);
#7373=AXIS2_PLACEMENT_3D('',#11074,#8644,#8645);
#7374=AXIS2_PLACEMENT_3D('',#11115,#8647,#8648);
#7375=AXIS2_PLACEMENT_3D('',#11138,#8650,#8651);
#7376=AXIS2_PLACEMENT_3D('',#11158,#8652,#8653);
#7377=AXIS2_PLACEMENT_3D('',#11161,#8654,#8655);
#7378=AXIS2_PLACEMENT_3D('',#11219,#8656,#8657);
#7379=AXIS2_PLACEMENT_3D('',#11260,#8659,#8660);
#7380=AXIS2_PLACEMENT_3D('',#11316,#8661,#8662);
#7381=AXIS2_PLACEMENT_3D('',#11320,#8664,#8665);
#7382=AXIS2_PLACEMENT_3D('',#11322,#8667,#8668);
#7383=AXIS2_PLACEMENT_3D('',#11325,#8669,#8670);
#7384=AXIS2_PLACEMENT_3D('',#11328,#8673,#8674);
#7385=AXIS2_PLACEMENT_3D('',#11331,#8675,#8676);
#7386=AXIS2_PLACEMENT_3D('',#11411,#8677,#8678);
#7387=AXIS2_PLACEMENT_3D('',#11414,#8679,#8680);
#7388=AXIS2_PLACEMENT_3D('',#11425,#8683,#8684);
#7389=AXIS2_PLACEMENT_3D('',#11427,#8686,#8687);
#7390=AXIS2_PLACEMENT_3D('',#11436,#8692,#8693);
#7391=AXIS2_PLACEMENT_3D('',#11437,#8694,#8695);
#7392=AXIS2_PLACEMENT_3D('',#11438,#8696,#8697);
#7393=AXIS2_PLACEMENT_3D('',#11443,#8699,#8700);
#7394=AXIS2_PLACEMENT_3D('',#11446,#8702,#8703);
#7395=AXIS2_PLACEMENT_3D('',#11447,#8704,#8705);
#7396=AXIS2_PLACEMENT_3D('',#11453,#8709,#8710);
#7397=AXIS2_PLACEMENT_3D('',#11455,#8711,#8712);
#7398=AXIS2_PLACEMENT_3D('',#11456,#8713,#8714);
#7399=AXIS2_PLACEMENT_3D('',#11457,#8715,#8716);
#7400=AXIS2_PLACEMENT_3D('',#11459,#8718,#8719);
#7401=AXIS2_PLACEMENT_3D('',#11461,#8720,#8721);
#7402=AXIS2_PLACEMENT_3D('',#11462,#8722,#8723);
#7403=AXIS2_PLACEMENT_3D('',#11464,#8725,#8726);
#7404=AXIS2_PLACEMENT_3D('',#11465,#8727,#8728);
#7405=AXIS2_PLACEMENT_3D('',#11466,#8729,#8730);
#7406=AXIS2_PLACEMENT_3D('',#11472,#8734,#8735);
#7407=AXIS2_PLACEMENT_3D('',#11477,#8737,#8738);
#7408=AXIS2_PLACEMENT_3D('',#11483,#8742,#8743);
#7409=AXIS2_PLACEMENT_3D('',#11484,#8744,#8745);
#7410=AXIS2_PLACEMENT_3D('',#11488,#8748,#8749);
#7411=AXIS2_PLACEMENT_3D('',#11491,#8751,#8752);
#7412=AXIS2_PLACEMENT_3D('',#11493,#8753,#8754);
#7413=AXIS2_PLACEMENT_3D('',#11495,#8756,#8757);
#7414=AXIS2_PLACEMENT_3D('',#11505,#8763,#8764);
#7415=AXIS2_PLACEMENT_3D('',#11515,#8770,#8771);
#7416=AXIS2_PLACEMENT_3D('',#11521,#8775,#8776);
#7417=AXIS2_PLACEMENT_3D('',#11530,#8781,#8782);
#7418=AXIS2_PLACEMENT_3D('',#11531,#8783,#8784);
#7419=AXIS2_PLACEMENT_3D('',#11532,#8785,#8786);
#7420=AXIS2_PLACEMENT_3D('',#11533,#8787,#8788);
#7421=AXIS2_PLACEMENT_3D('',#11534,#8789,#8790);
#7422=AXIS2_PLACEMENT_3D('',#11535,#8791,#8792);
#7423=AXIS2_PLACEMENT_3D('',#11536,#8793,#8794);
#7424=AXIS2_PLACEMENT_3D('',#11537,#8795,#8796);
#7425=AXIS2_PLACEMENT_3D('',#11538,#8797,#8798);
#7426=AXIS2_PLACEMENT_3D('',#11539,#8799,#8800);
#7427=AXIS2_PLACEMENT_3D('',#11540,#8801,#8802);
#7428=AXIS2_PLACEMENT_3D('',#11541,#8803,#8804);
#7429=AXIS2_PLACEMENT_3D('',#11542,#8805,#8806);
#7430=AXIS2_PLACEMENT_3D('',#11543,#8807,#8808);
#7431=AXIS2_PLACEMENT_3D('',#11544,#8809,#8810);
#7432=AXIS2_PLACEMENT_3D('',#11545,#8811,#8812);
#7433=AXIS2_PLACEMENT_3D('',#11546,#8813,#8814);
#7434=AXIS2_PLACEMENT_3D('',#11547,#8815,#8816);
#7435=AXIS2_PLACEMENT_3D('',#11548,#8817,#8818);
#7436=AXIS2_PLACEMENT_3D('',#11557,#8823,#8824);
#7437=AXIS2_PLACEMENT_3D('',#11560,#8826,#8827);
#7438=AXIS2_PLACEMENT_3D('',#11562,#8828,#8829);
#7439=AXIS2_PLACEMENT_3D('',#11564,#8831,#8832);
#7440=AXIS2_PLACEMENT_3D('',#11568,#8835,#8836);
#7441=AXIS2_PLACEMENT_3D('',#11569,#8837,#8838);
#7442=AXIS2_PLACEMENT_3D('',#11572,#8840,#8841);
#7443=AXIS2_PLACEMENT_3D('',#11573,#8842,#8843);
#7444=AXIS2_PLACEMENT_3D('',#11575,#8845,#8846);
#7445=AXIS2_PLACEMENT_3D('',#11576,#8847,#8848);
#7446=AXIS2_PLACEMENT_3D('',#11577,#8849,#8850);
#7447=AXIS2_PLACEMENT_3D('',#11578,#8851,#8852);
#7448=AXIS2_PLACEMENT_3D('',#11579,#8853,#8854);
#7449=AXIS2_PLACEMENT_3D('',#11580,#8855,#8856);
#7450=AXIS2_PLACEMENT_3D('',#11582,#8858,#8859);
#7451=AXIS2_PLACEMENT_3D('',#11584,#8861,#8862);
#7452=AXIS2_PLACEMENT_3D('',#11585,#8863,#8864);
#7453=AXIS2_PLACEMENT_3D('',#11586,#8865,#8866);
#7454=AXIS2_PLACEMENT_3D('',#11587,#8867,#8868);
#7455=AXIS2_PLACEMENT_3D('',#11588,#8869,#8870);
#7456=AXIS2_PLACEMENT_3D('',#11590,#8871,#8872);
#7457=AXIS2_PLACEMENT_3D('',#11593,#8874,#8875);
#7458=AXIS2_PLACEMENT_3D('',#11594,#8876,#8877);
#7459=AXIS2_PLACEMENT_3D('',#11596,#8878,#8879);
#7460=AXIS2_PLACEMENT_3D('',#11599,#8881,#8882);
#7461=AXIS2_PLACEMENT_3D('',#11600,#8883,#8884);
#7462=AXIS2_PLACEMENT_3D('',#11602,#8885,#8886);
#7463=AXIS2_PLACEMENT_3D('',#11605,#8888,#8889);
#7464=AXIS2_PLACEMENT_3D('',#11606,#8890,#8891);
#7465=AXIS2_PLACEMENT_3D('',#11615,#8896,#8897);
#7466=AXIS2_PLACEMENT_3D('',#11616,#8898,#8899);
#7467=AXIS2_PLACEMENT_3D('',#11619,#8900,#8901);
#7468=AXIS2_PLACEMENT_3D('',#11622,#8904,#8905);
#7469=AXIS2_PLACEMENT_3D('',#11626,#8908,#8909);
#7470=AXIS2_PLACEMENT_3D('',#11629,#8911,#8912);
#7471=AXIS2_PLACEMENT_3D('',#11630,#8913,#8914);
#7472=AXIS2_PLACEMENT_3D('',#11632,#8916,#8917);
#7473=AXIS2_PLACEMENT_3D('',#11633,#8918,#8919);
#7474=AXIS2_PLACEMENT_3D('',#11634,#8920,#8921);
#7475=AXIS2_PLACEMENT_3D('',#11635,#8922,#8923);
#7476=AXIS2_PLACEMENT_3D('',#11637,#8924,#8925);
#7477=AXIS2_PLACEMENT_3D('',#11640,#8927,#8928);
#7478=AXIS2_PLACEMENT_3D('',#11641,#8929,#8930);
#7479=AXIS2_PLACEMENT_3D('',#11644,#8931,#8932);
#7480=AXIS2_PLACEMENT_3D('',#11648,#8934,#8935);
#7481=AXIS2_PLACEMENT_3D('',#11650,#8937,#8938);
#7482=AXIS2_PLACEMENT_3D('',#11652,#8939,#8940);
#7483=AXIS2_PLACEMENT_3D('',#11655,#8942,#8943);
#7484=AXIS2_PLACEMENT_3D('',#11656,#8944,#8945);
#7485=AXIS2_PLACEMENT_3D('',#11665,#8950,#8951);
#7486=AXIS2_PLACEMENT_3D('',#11666,#8952,#8953);
#7487=AXIS2_PLACEMENT_3D('',#11669,#8956,#8957);
#7488=AXIS2_PLACEMENT_3D('',#11671,#8959,#8960);
#7489=AXIS2_PLACEMENT_3D('',#11673,#8962,#8963);
#7490=AXIS2_PLACEMENT_3D('',#11674,#8964,#8965);
#7491=AXIS2_PLACEMENT_3D('',#11675,#8966,#8967);
#7492=AXIS2_PLACEMENT_3D('',#11676,#8968,#8969);
#7493=AXIS2_PLACEMENT_3D('',#11677,#8970,#8971);
#7494=AXIS2_PLACEMENT_3D('',#11678,#8972,#8973);
#7495=AXIS2_PLACEMENT_3D('',#11680,#8974,#8975);
#7496=AXIS2_PLACEMENT_3D('',#11683,#8977,#8978);
#7497=AXIS2_PLACEMENT_3D('',#11684,#8979,#8980);
#7498=AXIS2_PLACEMENT_3D('',#11686,#8981,#8982);
#7499=AXIS2_PLACEMENT_3D('',#11689,#8984,#8985);
#7500=AXIS2_PLACEMENT_3D('',#11690,#8986,#8987);
#7501=AXIS2_PLACEMENT_3D('',#11692,#8988,#8989);
#7502=AXIS2_PLACEMENT_3D('',#11695,#8991,#8992);
#7503=AXIS2_PLACEMENT_3D('',#11696,#8993,#8994);
#7504=AXIS2_PLACEMENT_3D('',#11705,#8999,#9000);
#7505=AXIS2_PLACEMENT_3D('',#11706,#9001,#9002);
#7506=AXIS2_PLACEMENT_3D('',#11709,#9003,#9004);
#7507=AXIS2_PLACEMENT_3D('',#11712,#9007,#9008);
#7508=AXIS2_PLACEMENT_3D('',#11716,#9011,#9012);
#7509=AXIS2_PLACEMENT_3D('',#11719,#9014,#9015);
#7510=AXIS2_PLACEMENT_3D('',#11720,#9016,#9017);
#7511=AXIS2_PLACEMENT_3D('',#11722,#9019,#9020);
#7512=AXIS2_PLACEMENT_3D('',#11723,#9021,#9022);
#7513=AXIS2_PLACEMENT_3D('',#11724,#9023,#9024);
#7514=AXIS2_PLACEMENT_3D('',#11725,#9025,#9026);
#7515=AXIS2_PLACEMENT_3D('',#11727,#9027,#9028);
#7516=AXIS2_PLACEMENT_3D('',#11730,#9030,#9031);
#7517=AXIS2_PLACEMENT_3D('',#11731,#9032,#9033);
#7518=AXIS2_PLACEMENT_3D('',#11734,#9034,#9035);
#7519=AXIS2_PLACEMENT_3D('',#11738,#9037,#9038);
#7520=AXIS2_PLACEMENT_3D('',#11740,#9040,#9041);
#7521=AXIS2_PLACEMENT_3D('',#11742,#9042,#9043);
#7522=AXIS2_PLACEMENT_3D('',#11745,#9045,#9046);
#7523=AXIS2_PLACEMENT_3D('',#11746,#9047,#9048);
#7524=AXIS2_PLACEMENT_3D('',#11755,#9053,#9054);
#7525=AXIS2_PLACEMENT_3D('',#11756,#9055,#9056);
#7526=AXIS2_PLACEMENT_3D('',#11759,#9059,#9060);
#7527=AXIS2_PLACEMENT_3D('',#11761,#9062,#9063);
#7528=AXIS2_PLACEMENT_3D('',#11763,#9065,#9066);
#7529=AXIS2_PLACEMENT_3D('',#11764,#9067,#9068);
#7530=AXIS2_PLACEMENT_3D('',#11765,#9069,#9070);
#7531=AXIS2_PLACEMENT_3D('',#11766,#9071,#9072);
#7532=AXIS2_PLACEMENT_3D('',#11767,#9073,#9074);
#7533=AXIS2_PLACEMENT_3D('',#11768,#9075,#9076);
#7534=AXIS2_PLACEMENT_3D('',#11770,#9077,#9078);
#7535=AXIS2_PLACEMENT_3D('',#11773,#9080,#9081);
#7536=AXIS2_PLACEMENT_3D('',#11774,#9082,#9083);
#7537=AXIS2_PLACEMENT_3D('',#11776,#9084,#9085);
#7538=AXIS2_PLACEMENT_3D('',#11779,#9087,#9088);
#7539=AXIS2_PLACEMENT_3D('',#11780,#9089,#9090);
#7540=AXIS2_PLACEMENT_3D('',#11782,#9091,#9092);
#7541=AXIS2_PLACEMENT_3D('',#11785,#9094,#9095);
#7542=AXIS2_PLACEMENT_3D('',#11786,#9096,#9097);
#7543=AXIS2_PLACEMENT_3D('',#11795,#9102,#9103);
#7544=AXIS2_PLACEMENT_3D('',#11796,#9104,#9105);
#7545=AXIS2_PLACEMENT_3D('',#11799,#9106,#9107);
#7546=AXIS2_PLACEMENT_3D('',#11802,#9110,#9111);
#7547=AXIS2_PLACEMENT_3D('',#11806,#9114,#9115);
#7548=AXIS2_PLACEMENT_3D('',#11809,#9117,#9118);
#7549=AXIS2_PLACEMENT_3D('',#11810,#9119,#9120);
#7550=AXIS2_PLACEMENT_3D('',#11812,#9122,#9123);
#7551=AXIS2_PLACEMENT_3D('',#11813,#9124,#9125);
#7552=AXIS2_PLACEMENT_3D('',#11814,#9126,#9127);
#7553=AXIS2_PLACEMENT_3D('',#11815,#9128,#9129);
#7554=AXIS2_PLACEMENT_3D('',#11817,#9130,#9131);
#7555=AXIS2_PLACEMENT_3D('',#11820,#9133,#9134);
#7556=AXIS2_PLACEMENT_3D('',#11821,#9135,#9136);
#7557=AXIS2_PLACEMENT_3D('',#11824,#9137,#9138);
#7558=AXIS2_PLACEMENT_3D('',#11828,#9140,#9141);
#7559=AXIS2_PLACEMENT_3D('',#11830,#9143,#9144);
#7560=AXIS2_PLACEMENT_3D('',#11832,#9145,#9146);
#7561=AXIS2_PLACEMENT_3D('',#11835,#9148,#9149);
#7562=AXIS2_PLACEMENT_3D('',#11836,#9150,#9151);
#7563=AXIS2_PLACEMENT_3D('',#11845,#9156,#9157);
#7564=AXIS2_PLACEMENT_3D('',#11846,#9158,#9159);
#7565=AXIS2_PLACEMENT_3D('',#11849,#9162,#9163);
#7566=AXIS2_PLACEMENT_3D('',#11851,#9165,#9166);
#7567=AXIS2_PLACEMENT_3D('',#11853,#9168,#9169);
#7568=AXIS2_PLACEMENT_3D('',#11854,#9170,#9171);
#7569=AXIS2_PLACEMENT_3D('',#11855,#9172,#9173);
#7570=AXIS2_PLACEMENT_3D('',#11857,#9174,#9175);
#7571=AXIS2_PLACEMENT_3D('',#11860,#9177,#9178);
#7572=AXIS2_PLACEMENT_3D('',#11861,#9179,#9180);
#7573=AXIS2_PLACEMENT_3D('',#11863,#9181,#9182);
#7574=AXIS2_PLACEMENT_3D('',#11866,#9184,#9185);
#7575=AXIS2_PLACEMENT_3D('',#11867,#9186,#9187);
#7576=AXIS2_PLACEMENT_3D('',#11869,#9188,#9189);
#7577=AXIS2_PLACEMENT_3D('',#11872,#9191,#9192);
#7578=AXIS2_PLACEMENT_3D('',#11873,#9193,#9194);
#7579=AXIS2_PLACEMENT_3D('',#11882,#9199,#9200);
#7580=AXIS2_PLACEMENT_3D('',#11892,#9206,#9207);
#7581=AXIS2_PLACEMENT_3D('',#11898,#9211,#9212);
#7582=AXIS2_PLACEMENT_3D('',#11908,#9218,#9219);
#7583=AXIS2_PLACEMENT_3D('',#11911,#9222,#9223);
#7584=AXIS2_PLACEMENT_3D('',#11912,#9224,#9225);
#7585=AXIS2_PLACEMENT_3D('',#11920,#9230,#9231);
#7586=AXIS2_PLACEMENT_3D('',#11928,#9236,#9237);
#7587=AXIS2_PLACEMENT_3D('',#11930,#9239,#9240);
#7588=AXIS2_PLACEMENT_3D('',#11932,#9242,#9243);
#7589=AXIS2_PLACEMENT_3D('',#11934,#9245,#9246);
#7590=AXIS2_PLACEMENT_3D('',#11935,#9247,#9248);
#7591=AXIS2_PLACEMENT_3D('',#11936,#9249,#9250);
#7592=AXIS2_PLACEMENT_3D('',#11937,#9251,#9252);
#7593=AXIS2_PLACEMENT_3D('',#11938,#9253,#9254);
#7594=AXIS2_PLACEMENT_3D('',#11939,#9255,#9256);
#7595=AXIS2_PLACEMENT_3D('',#11940,#9257,#9258);
#7596=AXIS2_PLACEMENT_3D('',#11941,#9259,#9260);
#7597=AXIS2_PLACEMENT_3D('',#11943,#9261,#9262);
#7598=AXIS2_PLACEMENT_3D('',#11990,#9264,#9265);
#7599=AXIS2_PLACEMENT_3D('',#12018,#9267,#9268);
#7600=AXIS2_PLACEMENT_3D('',#12067,#9269,#9270);
#7601=AXIS2_PLACEMENT_3D('',#12069,#9271,#9272);
#7602=AXIS2_PLACEMENT_3D('',#12142,#9273,#9274);
#7603=AXIS2_PLACEMENT_3D('',#12145,#9275,#9276);
#7604=AXIS2_PLACEMENT_3D('',#12149,#9278,#9279);
#7605=AXIS2_PLACEMENT_3D('',#12151,#9281,#9282);
#7606=AXIS2_PLACEMENT_3D('',#12160,#9287,#9288);
#7607=AXIS2_PLACEMENT_3D('',#12163,#9291,#9292);
#7608=AXIS2_PLACEMENT_3D('',#12165,#9294,#9295);
#7609=AXIS2_PLACEMENT_3D('',#12167,#9297,#9298);
#7610=AXIS2_PLACEMENT_3D('',#12168,#9299,#9300);
#7611=AXIS2_PLACEMENT_3D('',#12169,#9301,#9302);
#7612=AXIS2_PLACEMENT_3D('',#12170,#9303,#9304);
#7613=AXIS2_PLACEMENT_3D('',#12171,#9305,#9306);
#7614=AXIS2_PLACEMENT_3D('',#12172,#9307,#9308);
#7615=AXIS2_PLACEMENT_3D('',#12173,#9309,#9310);
#7616=AXIS2_PLACEMENT_3D('',#12174,#9311,#9312);
#7617=AXIS2_PLACEMENT_3D('',#12175,#9313,#9314);
#7618=AXIS2_PLACEMENT_3D('',#12176,#9315,#9316);
#7619=AXIS2_PLACEMENT_3D('',#12177,#9317,#9318);
#7620=AXIS2_PLACEMENT_3D('',#12179,#9319,#9320);
#7621=AXIS2_PLACEMENT_3D('',#12182,#9322,#9323);
#7622=AXIS2_PLACEMENT_3D('',#12183,#9324,#9325);
#7623=AXIS2_PLACEMENT_3D('',#12185,#9326,#9327);
#7624=AXIS2_PLACEMENT_3D('',#12188,#9329,#9330);
#7625=AXIS2_PLACEMENT_3D('',#12189,#9331,#9332);
#7626=AXIS2_PLACEMENT_3D('',#12191,#9333,#9334);
#7627=AXIS2_PLACEMENT_3D('',#12194,#9336,#9337);
#7628=AXIS2_PLACEMENT_3D('',#12195,#9338,#9339);
#7629=AXIS2_PLACEMENT_3D('',#12197,#9340,#9341);
#7630=AXIS2_PLACEMENT_3D('',#12200,#9343,#9344);
#7631=AXIS2_PLACEMENT_3D('',#12201,#9345,#9346);
#7632=AXIS2_PLACEMENT_3D('',#12203,#9347,#9348);
#7633=AXIS2_PLACEMENT_3D('',#12205,#9349,#9350);
#7634=AXIS2_PLACEMENT_3D('',#12207,#9351,#9352);
#7635=AXIS2_PLACEMENT_3D('',#12209,#9353,#9354);
#7636=AXIS2_PLACEMENT_3D('',#12210,#9355,#9356);
#7637=AXIS2_PLACEMENT_3D('',#12212,#9357,#9358);
#7638=AXIS2_PLACEMENT_3D('',#12214,#9359,#9360);
#7639=AXIS2_PLACEMENT_3D('',#12215,#9361,#9362);
#7640=AXIS2_PLACEMENT_3D('',#12218,#9363,#9364);
#7641=AXIS2_PLACEMENT_3D('',#12220,#9365,#9366);
#7642=AXIS2_PLACEMENT_3D('',#12222,#9367,#9368);
#7643=AXIS2_PLACEMENT_3D('',#12223,#9369,#9370);
#7644=AXIS2_PLACEMENT_3D('',#12226,#9371,#9372);
#7645=AXIS2_PLACEMENT_3D('',#12228,#9373,#9374);
#7646=AXIS2_PLACEMENT_3D('',#12230,#9375,#9376);
#7647=AXIS2_PLACEMENT_3D('',#12231,#9377,#9378);
#7648=AXIS2_PLACEMENT_3D('',#12232,#9379,#9380);
#7649=AXIS2_PLACEMENT_3D('',#12241,#9385,#9386);
#7650=AXIS2_PLACEMENT_3D('',#12247,#9390,#9391);
#7651=AXIS2_PLACEMENT_3D('',#12251,#9394,#9395);
#7652=AXIS2_PLACEMENT_3D('',#12255,#9398,#9399);
#7653=AXIS2_PLACEMENT_3D('',#12257,#9401,#9402);
#7654=AXIS2_PLACEMENT_3D('',#12258,#9403,#9404);
#7655=AXIS2_PLACEMENT_3D('',#12262,#9407,#9408);
#7656=AXIS2_PLACEMENT_3D('',#12266,#9411,#9412);
#7657=AXIS2_PLACEMENT_3D('',#12268,#9414,#9415);
#7658=AXIS2_PLACEMENT_3D('',#12269,#9416,#9417);
#7659=AXIS2_PLACEMENT_3D('',#12280,#9424,#9425);
#7660=AXIS2_PLACEMENT_3D('',#12284,#9428,#9429);
#7661=AXIS2_PLACEMENT_3D('',#12293,#9435,#9436);
#7662=AXIS2_PLACEMENT_3D('',#12294,#9437,#9438);
#7663=AXIS2_PLACEMENT_3D('',#12296,#9440,#9441);
#7664=AXIS2_PLACEMENT_3D('',#12299,#9444,#9445);
#7665=AXIS2_PLACEMENT_3D('',#12300,#9446,#9447);
#7666=AXIS2_PLACEMENT_3D('',#12301,#9448,#9449);
#7667=AXIS2_PLACEMENT_3D('',#12302,#9450,#9451);
#7668=AXIS2_PLACEMENT_3D('',#12304,#9452,#9453);
#7669=AXIS2_PLACEMENT_3D('',#12307,#9455,#9456);
#7670=AXIS2_PLACEMENT_3D('',#12308,#9457,#9458);
#7671=AXIS2_PLACEMENT_3D('',#12310,#9459,#9460);
#7672=AXIS2_PLACEMENT_3D('',#12351,#9462,#9463);
#7673=AXIS2_PLACEMENT_3D('',#12374,#9465,#9466);
#7674=AXIS2_PLACEMENT_3D('',#12394,#9467,#9468);
#7675=AXIS2_PLACEMENT_3D('',#12402,#9472,#9473);
#7676=AXIS2_PLACEMENT_3D('',#12403,#9474,#9475);
#7677=AXIS2_PLACEMENT_3D('',#12407,#9477,#9478);
#7678=AXIS2_PLACEMENT_3D('',#12442,#9481,#9482);
#7679=AXIS2_PLACEMENT_3D('',#12443,#9483,#9484);
#7680=AXIS2_PLACEMENT_3D('',#12445,#9485,#9486);
#7681=AXIS2_PLACEMENT_3D('',#12449,#9488,#9489);
#7682=AXIS2_PLACEMENT_3D('',#12478,#9491,#9492);
#7683=AXIS2_PLACEMENT_3D('',#12479,#9493,#9494);
#7684=AXIS2_PLACEMENT_3D('',#12485,#9495,#9496);
#7685=AXIS2_PLACEMENT_3D('',#12546,#9497,#9498);
#7686=AXIS2_PLACEMENT_3D('',#12550,#9499,#9500);
#7687=AXIS2_PLACEMENT_3D('',#12552,#9502,#9503);
#7688=AXIS2_PLACEMENT_3D('',#12554,#9505,#9506);
#7689=AXIS2_PLACEMENT_3D('',#12558,#9508,#9509);
#7690=AXIS2_PLACEMENT_3D('',#12559,#9510,#9511);
#7691=AXIS2_PLACEMENT_3D('',#12560,#9512,#9513);
#7692=AXIS2_PLACEMENT_3D('',#12564,#9516,#9517);
#7693=AXIS2_PLACEMENT_3D('',#12568,#9520,#9521);
#7694=AXIS2_PLACEMENT_3D('',#12570,#9523,#9524);
#7695=AXIS2_PLACEMENT_3D('',#12571,#9525,#9526);
#7696=AXIS2_PLACEMENT_3D('',#12577,#9530,#9531);
#7697=AXIS2_PLACEMENT_3D('',#12583,#9535,#9536);
#7698=AXIS2_PLACEMENT_3D('',#12586,#9539,#9540);
#7699=AXIS2_PLACEMENT_3D('',#12587,#9541,#9542);
#7700=AXIS2_PLACEMENT_3D('',#12588,#9543,#9544);
#7701=AXIS2_PLACEMENT_3D('',#12589,#9545,#9546);
#7702=AXIS2_PLACEMENT_3D('',#12591,#9547,#9548);
#7703=AXIS2_PLACEMENT_3D('',#12636,#9550,#9551);
#7704=AXIS2_PLACEMENT_3D('',#12661,#9553,#9554);
#7705=AXIS2_PLACEMENT_3D('',#12683,#9555,#9556);
#7706=AXIS2_PLACEMENT_3D('',#12705,#9557,#9558);
#7707=AXIS2_PLACEMENT_3D('',#12709,#9560,#9561);
#7708=AXIS2_PLACEMENT_3D('',#12713,#9563,#9564);
#7709=AXIS2_PLACEMENT_3D('',#12717,#9566,#9567);
#7710=AXIS2_PLACEMENT_3D('',#12720,#9569,#9570);
#7711=AXIS2_PLACEMENT_3D('',#12721,#9571,#9572);
#7712=AXIS2_PLACEMENT_3D('',#12723,#9573,#9574);
#7713=AXIS2_PLACEMENT_3D('',#12726,#9576,#9577);
#7714=AXIS2_PLACEMENT_3D('',#12727,#9578,#9579);
#7715=AXIS2_PLACEMENT_3D('',#12729,#9580,#9581);
#7716=AXIS2_PLACEMENT_3D('',#12732,#9583,#9584);
#7717=AXIS2_PLACEMENT_3D('',#12733,#9585,#9586);
#7718=AXIS2_PLACEMENT_3D('',#12735,#9587,#9588);
#7719=AXIS2_PLACEMENT_3D('',#12738,#9590,#9591);
#7720=AXIS2_PLACEMENT_3D('',#12739,#9592,#9593);
#7721=AXIS2_PLACEMENT_3D('',#12783,#9594,#9595);
#7722=AXIS2_PLACEMENT_3D('',#12830,#9596,#9597);
#7723=AXIS2_PLACEMENT_3D('',#12836,#9598,#9599);
#7724=AXIS2_PLACEMENT_3D('',#12840,#9602,#9603);
#7725=AXIS2_PLACEMENT_3D('',#12843,#9605,#9606);
#7726=AXIS2_PLACEMENT_3D('',#12844,#9607,#9608);
#7727=AXIS2_PLACEMENT_3D('',#12849,#9611,#9612);
#7728=AXIS2_PLACEMENT_3D('',#12850,#9613,#9614);
#7729=AXIS2_PLACEMENT_3D('',#12859,#9619,#9620);
#7730=AXIS2_PLACEMENT_3D('',#12861,#9621,#9622);
#7731=AXIS2_PLACEMENT_3D('',#12872,#9623,#9624);
#7732=AXIS2_PLACEMENT_3D('',#12875,#9625,#9626);
#7733=AXIS2_PLACEMENT_3D('',#12877,#9628,#9629);
#7734=AXIS2_PLACEMENT_3D('',#12881,#9631,#9632);
#7735=AXIS2_PLACEMENT_3D('',#12883,#9634,#9635);
#7736=AXIS2_PLACEMENT_3D('',#12886,#9638,#9639);
#7737=AXIS2_PLACEMENT_3D('',#12887,#9640,#9641);
#7738=AXIS2_PLACEMENT_3D('',#12890,#9642,#9643);
#7739=AXIS2_PLACEMENT_3D('',#12891,#9644,#9645);
#7740=AXIS2_PLACEMENT_3D('',#12897,#9649,#9650);
#7741=AXIS2_PLACEMENT_3D('',#12899,#9651,#9652);
#7742=AXIS2_PLACEMENT_3D('',#12901,#9653,#9654);
#7743=AXIS2_PLACEMENT_3D('',#12907,#9658,#9659);
#7744=AXIS2_PLACEMENT_3D('',#12909,#9661,#9662);
#7745=AXIS2_PLACEMENT_3D('',#12911,#9663,#9664);
#7746=AXIS2_PLACEMENT_3D('',#12917,#9668,#9669);
#7747=AXIS2_PLACEMENT_3D('',#12922,#9671,#9672);
#7748=AXIS2_PLACEMENT_3D('',#12928,#9676,#9677);
#7749=AXIS2_PLACEMENT_3D('',#12929,#9678,#9679);
#7750=AXIS2_PLACEMENT_3D('',#12933,#9682,#9683);
#7751=AXIS2_PLACEMENT_3D('',#12936,#9685,#9686);
#7752=AXIS2_PLACEMENT_3D('',#12938,#9687,#9688);
#7753=AXIS2_PLACEMENT_3D('',#12941,#9691,#9692);
#7754=AXIS2_PLACEMENT_3D('',#12942,#9693,#9694);
#7755=AXIS2_PLACEMENT_3D('',#12950,#9700,#9701);
#7756=AXIS2_PLACEMENT_3D('',#12957,#9706,#9707);
#7757=AXIS2_PLACEMENT_3D('',#12963,#9711,#9712);
#7758=AXIS2_PLACEMENT_3D('',#12965,#9714,#9715);
#7759=AXIS2_PLACEMENT_3D('',#12966,#9716,#9717);
#7760=AXIS2_PLACEMENT_3D('',#12967,#9718,#9719);
#7761=AXIS2_PLACEMENT_3D('',#12968,#9720,#9721);
#7762=AXIS2_PLACEMENT_3D('',#12969,#9722,#9723);
#7763=AXIS2_PLACEMENT_3D('',#12970,#9724,#9725);
#7764=AXIS2_PLACEMENT_3D('',#12971,#9726,#9727);
#7765=AXIS2_PLACEMENT_3D('',#12972,#9728,#9729);
#7766=AXIS2_PLACEMENT_3D('',#12973,#9730,#9731);
#7767=AXIS2_PLACEMENT_3D('',#12974,#9732,#9733);
#7768=AXIS2_PLACEMENT_3D('',#12975,#9734,#9735);
#7769=AXIS2_PLACEMENT_3D('',#12976,#9736,#9737);
#7770=AXIS2_PLACEMENT_3D('',#12977,#9738,#9739);
#7771=AXIS2_PLACEMENT_3D('',#12978,#9740,#9741);
#7772=AXIS2_PLACEMENT_3D('',#12982,#9745,#9746);
#7773=AXIS2_PLACEMENT_3D('',#12984,#9748,#9749);
#7774=AXIS2_PLACEMENT_3D('',#12985,#9750,#9751);
#7775=AXIS2_PLACEMENT_3D('',#12986,#9752,#9753);
#7776=AXIS2_PLACEMENT_3D('',#12987,#9754,#9755);
#7777=AXIS2_PLACEMENT_3D('',#13016,#9756,#9757);
#7778=AXIS2_PLACEMENT_3D('',#13018,#9758,#9759);
#7779=AXIS2_PLACEMENT_3D('',#13047,#9760,#9761);
#7780=AXIS2_PLACEMENT_3D('',#13048,#9762,#9763);
#7781=AXIS2_PLACEMENT_3D('',#13049,#9764,#9765);
#7782=AXIS2_PLACEMENT_3D('',#13050,#9766,#9767);
#7783=AXIS2_PLACEMENT_3D('',#13051,#9768,#9769);
#7784=AXIS2_PLACEMENT_3D('',#13052,#9770,#9771);
#7785=AXIS2_PLACEMENT_3D('',#13054,#9772,#9773);
#7786=AXIS2_PLACEMENT_3D('',#13057,#9775,#9776);
#7787=AXIS2_PLACEMENT_3D('',#13058,#9777,#9778);
#7788=AXIS2_PLACEMENT_3D('',#13060,#9779,#9780);
#7789=AXIS2_PLACEMENT_3D('',#13063,#9782,#9783);
#7790=AXIS2_PLACEMENT_3D('',#13064,#9784,#9785);
#7791=AXIS2_PLACEMENT_3D('',#13066,#9786,#9787);
#7792=AXIS2_PLACEMENT_3D('',#13069,#9789,#9790);
#7793=AXIS2_PLACEMENT_3D('',#13070,#9791,#9792);
#7794=AXIS2_PLACEMENT_3D('',#13079,#9797,#9798);
#7795=AXIS2_PLACEMENT_3D('',#13080,#9799,#9800);
#7796=AXIS2_PLACEMENT_3D('',#13083,#9801,#9802);
#7797=AXIS2_PLACEMENT_3D('',#13086,#9805,#9806);
#7798=AXIS2_PLACEMENT_3D('',#13090,#9809,#9810);
#7799=AXIS2_PLACEMENT_3D('',#13093,#9812,#9813);
#7800=AXIS2_PLACEMENT_3D('',#13094,#9814,#9815);
#7801=AXIS2_PLACEMENT_3D('',#13096,#9817,#9818);
#7802=AXIS2_PLACEMENT_3D('',#13097,#9819,#9820);
#7803=AXIS2_PLACEMENT_3D('',#13098,#9821,#9822);
#7804=AXIS2_PLACEMENT_3D('',#13099,#9823,#9824);
#7805=AXIS2_PLACEMENT_3D('',#13101,#9825,#9826);
#7806=AXIS2_PLACEMENT_3D('',#13104,#9828,#9829);
#7807=AXIS2_PLACEMENT_3D('',#13105,#9830,#9831);
#7808=AXIS2_PLACEMENT_3D('',#13108,#9832,#9833);
#7809=AXIS2_PLACEMENT_3D('',#13112,#9835,#9836);
#7810=AXIS2_PLACEMENT_3D('',#13114,#9838,#9839);
#7811=AXIS2_PLACEMENT_3D('',#13116,#9840,#9841);
#7812=AXIS2_PLACEMENT_3D('',#13119,#9843,#9844);
#7813=AXIS2_PLACEMENT_3D('',#13120,#9845,#9846);
#7814=AXIS2_PLACEMENT_3D('',#13129,#9851,#9852);
#7815=AXIS2_PLACEMENT_3D('',#13130,#9853,#9854);
#7816=AXIS2_PLACEMENT_3D('',#13133,#9857,#9858);
#7817=AXIS2_PLACEMENT_3D('',#13135,#9860,#9861);
#7818=AXIS2_PLACEMENT_3D('',#13137,#9863,#9864);
#7819=AXIS2_PLACEMENT_3D('',#13138,#9865,#9866);
#7820=AXIS2_PLACEMENT_3D('',#13139,#9867,#9868);
#7821=AXIS2_PLACEMENT_3D('',#13140,#9869,#9870);
#7822=AXIS2_PLACEMENT_3D('',#13141,#9871,#9872);
#7823=AXIS2_PLACEMENT_3D('',#13142,#9873,#9874);
#7824=AXIS2_PLACEMENT_3D('',#13143,#9875,#9876);
#7825=AXIS2_PLACEMENT_3D('',#13144,#9877,#9878);
#7826=AXIS2_PLACEMENT_3D('',#13145,#9879,#9880);
#7827=AXIS2_PLACEMENT_3D('',#13146,#9881,#9882);
#7828=AXIS2_PLACEMENT_3D('',#13147,#9883,#9884);
#7829=DIRECTION('axis',(0.,0.,1.));
#7830=DIRECTION('refdir',(1.,0.,0.));
#7831=DIRECTION('axis',(0.,0.,1.));
#7832=DIRECTION('refdir',(1.,0.,0.));
#7833=DIRECTION('center_axis',(0.,0.,1.));
#7834=DIRECTION('ref_axis',(1.,0.,0.));
#7835=DIRECTION('center_axis',(0.,0.,-1.));
#7836=DIRECTION('ref_axis',(1.,0.,0.));
#7837=DIRECTION('center_axis',(-0.641775581367837,0.76689249778569,-5.56651583653725E-16));
#7838=DIRECTION('ref_axis',(-0.76689249778569,-0.641775581367837,2.9218149482617E-31));
#7839=DIRECTION('center_axis',(0.,0.,1.));
#7840=DIRECTION('ref_axis',(1.,0.,0.));
#7841=DIRECTION('center_axis',(0.984885527325901,0.173206518537793,0.));
#7842=DIRECTION('ref_axis',(0.173206518537793,-0.984885527325901,0.));
#7843=DIRECTION('center_axis',(0.,0.,1.));
#7844=DIRECTION('ref_axis',(1.,0.,0.));
#7845=DIRECTION('center_axis',(0.,0.,-1.));
#7846=DIRECTION('ref_axis',(1.,0.,0.));
#7847=DIRECTION('center_axis',(-0.641775581367838,0.76689249778569,0.));
#7848=DIRECTION('ref_axis',(-0.76689249778569,-0.641775581367838,0.));
#7849=DIRECTION('center_axis',(0.,0.,1.));
#7850=DIRECTION('ref_axis',(1.,0.,0.));
#7851=DIRECTION('center_axis',(-0.984885527325901,-0.173206518537793,0.));
#7852=DIRECTION('ref_axis',(0.173206518537793,-0.984885527325901,0.));
#7853=DIRECTION('center_axis',(1.,0.,0.));
#7854=DIRECTION('ref_axis',(0.,1.,6.88338275267597E-15));
#7855=DIRECTION('center_axis',(0.,0.,1.));
#7856=DIRECTION('ref_axis',(-1.,6.93889390390722E-15,0.));
#7857=DIRECTION('center_axis',(0.,1.,6.93889390390722E-15));
#7858=DIRECTION('ref_axis',(0.,-6.93889390390722E-15,1.));
#7859=DIRECTION('center_axis',(-0.992279004699137,-0.124025710372042,0.));
#7860=DIRECTION('ref_axis',(-0.124025710372042,0.992279004699137,0.));
#7861=DIRECTION('center_axis',(0.0933963198450884,0.961399932042651,0.25881904510252));
#7862=DIRECTION('ref_axis',(2.98017618614267E-17,-0.259955306903251,0.965620649330179));
#7863=DIRECTION('center_axis',(-0.0933963198450884,-0.961399932042651,-0.25881904510252));
#7864=DIRECTION('ref_axis',(-3.0291317207828E-17,0.259955306903251,-0.965620649330179));
#7865=DIRECTION('',(0.0933963198450884,0.961399932042651,0.25881904510252));
#7866=DIRECTION('center_axis',(0.0933963198450884,0.961399932042651,0.25881904510252));
#7867=DIRECTION('ref_axis',(2.98017618614267E-17,-0.259955306903251,0.965620649330179));
#7868=DIRECTION('center_axis',(-1.,0.,0.));
#7869=DIRECTION('ref_axis',(0.,0.,1.));
#7870=DIRECTION('center_axis',(1.,0.,0.));
#7871=DIRECTION('ref_axis',(0.,0.,-1.));
#7872=DIRECTION('',(-1.,0.,0.));
#7873=DIRECTION('center_axis',(-1.,0.,0.));
#7874=DIRECTION('ref_axis',(0.,0.,1.));
#7875=DIRECTION('center_axis',(0.,0.,-1.));
#7876=DIRECTION('ref_axis',(-1.,0.,0.));
#7877=DIRECTION('center_axis',(0.,0.,-1.));
#7878=DIRECTION('ref_axis',(1.,0.,0.));
#7879=DIRECTION('',(0.,0.,-1.));
#7880=DIRECTION('center_axis',(0.,0.,1.));
#7881=DIRECTION('ref_axis',(1.,0.,0.));
#7882=DIRECTION('',(0.,0.,-1.));
#7883=DIRECTION('center_axis',(-0.0250254684785304,-0.257606335394166,0.965925826289068));
#7884=DIRECTION('ref_axis',(1.03108140825845E-18,-0.96622843558427,-0.257687039387652));
#7885=DIRECTION('',(0.995314449491629,-0.0966909852735815,0.));
#7886=DIRECTION('',(-0.0933963198450936,-0.96139993204265,-0.258819045102522));
#7887=DIRECTION('',(0.995314449491629,-0.0966909852735815,0.));
#7888=DIRECTION('center_axis',(0.0250254684785293,0.257606335394166,-0.965925826289068));
#7889=DIRECTION('ref_axis',(0.0933963198489319,0.961399932042277,0.258819045102523));
#7890=DIRECTION('center_axis',(0.0933963198450884,0.961399932042651,0.25881904510252));
#7891=DIRECTION('ref_axis',(1.37707821742972E-18,-0.259955306903251,0.965620649330179));
#7892=DIRECTION('',(0.995314449491629,-0.0966909852735815,0.));
#7893=DIRECTION('center_axis',(0.0933963198450884,0.961399932042651,0.25881904510252));
#7894=DIRECTION('ref_axis',(3.43206474624895E-18,-0.259955306903251,0.965620649330179));
#7895=DIRECTION('',(-0.933373647950443,-0.00593445768887964,0.358857096242532));
#7896=DIRECTION('center_axis',(0.0933963198450885,0.961399932042651,0.25881904510252));
#7897=DIRECTION('ref_axis',(-2.92726432357018E-17,-0.259955306903251,0.965620649330179));
#7898=DIRECTION('',(0.917438844473794,-0.184084480291559,0.352730592331281));
#7899=DIRECTION('center_axis',(0.0933963198450884,0.961399932042651,0.25881904510252));
#7900=DIRECTION('ref_axis',(3.43206474624895E-18,-0.259955306903251,0.965620649330179));
#7901=DIRECTION('center_axis',(-0.0933963198450819,-0.961399932042651,-0.25881904510252));
#7902=DIRECTION('ref_axis',(0.0250254684833587,0.257606335393695,-0.965925826289068));
#7903=DIRECTION('center_axis',(0.0250254684785304,0.257606335394166,-0.965925826289068));
#7904=DIRECTION('ref_axis',(-1.38210229589347E-18,0.96622843558427,0.257687039387653));
#7905=DIRECTION('',(0.995314449491629,-0.0966909852735815,0.));
#7906=DIRECTION('',(0.0933963198450826,0.961399932042651,0.258819045102522));
#7907=DIRECTION('center_axis',(-0.0250254684785248,-0.257606335394166,0.965925826289068));
#7908=DIRECTION('ref_axis',(-0.0933963198403989,-0.961399932043106,-0.258819045102522));
#7909=DIRECTION('center_axis',(-0.0933963198450884,-0.961399932042651,-0.25881904510252));
#7910=DIRECTION('ref_axis',(2.59294345608955E-18,0.259955306903251,-0.965620649330179));
#7911=DIRECTION('',(-0.933373647950443,-0.00593445768887968,0.358857096242532));
#7912=DIRECTION('center_axis',(-0.0933963198450884,-0.961399932042651,-0.25881904510252));
#7913=DIRECTION('ref_axis',(9.33705359754526E-19,0.259955306903251,-0.965620649330179));
#7914=DIRECTION('center_axis',(0.0933963198450923,0.961399932042651,0.25881904510252));
#7915=DIRECTION('ref_axis',(-0.0250254684771762,-0.257606335394296,0.965925826289068));
#7916=DIRECTION('center_axis',(-0.0933963198450884,-0.961399932042651,-0.25881904510252));
#7917=DIRECTION('ref_axis',(9.33705359754526E-19,0.259955306903251,-0.965620649330179));
#7918=DIRECTION('',(0.917438844473794,-0.184084480291559,0.352730592331281));
#7919=DIRECTION('center_axis',(0.0933963198450884,0.961399932042651,0.25881904510252));
#7920=DIRECTION('ref_axis',(2.17503870714762E-17,0.259955306903251,-0.965620649330179));
#7921=DIRECTION('center_axis',(0.,0.,-1.));
#7922=DIRECTION('ref_axis',(-1.,0.,0.));
#7923=DIRECTION('center_axis',(0.,0.,-1.));
#7924=DIRECTION('ref_axis',(1.,5.35536752134463E-15,0.));
#7925=DIRECTION('',(0.,0.,-1.));
#7926=DIRECTION('center_axis',(0.,0.,1.));
#7927=DIRECTION('ref_axis',(1.,0.,0.));
#7928=DIRECTION('',(0.,0.,1.));
#7929=DIRECTION('',(0.,0.,1.));
#7930=DIRECTION('center_axis',(0.,0.,-1.));
#7931=DIRECTION('ref_axis',(1.,0.,0.));
#7932=DIRECTION('',(0.,0.,1.));
#7933=DIRECTION('center_axis',(0.,0.,1.));
#7934=DIRECTION('ref_axis',(1.,0.,0.));
#7935=DIRECTION('center_axis',(0.,0.,1.));
#7936=DIRECTION('ref_axis',(1.,0.,0.));
#7937=DIRECTION('',(-2.7390370673318E-16,1.,0.));
#7938=DIRECTION('',(-1.,0.,0.));
#7939=DIRECTION('',(0.,1.,0.));
#7940=DIRECTION('',(1.,0.,0.));
#7941=DIRECTION('center_axis',(0.,0.,-1.));
#7942=DIRECTION('ref_axis',(0.939389765090764,-0.342851089020758,0.));
#7943=DIRECTION('',(0.,0.,1.));
#7944=DIRECTION('center_axis',(1.22464679914735E-16,-1.,0.));
#7945=DIRECTION('ref_axis',(1.,1.22464679914735E-16,0.));
#7946=DIRECTION('',(1.,1.22464679914735E-16,0.));
#7947=DIRECTION('',(0.,0.,-1.));
#7948=DIRECTION('',(-1.,-1.22464679914735E-16,0.));
#7949=DIRECTION('',(0.,0.,1.));
#7950=DIRECTION('center_axis',(1.,2.31296463463574E-16,0.));
#7951=DIRECTION('ref_axis',(-2.31296463463574E-16,1.,0.));
#7952=DIRECTION('',(-2.31296463463574E-16,1.,0.));
#7953=DIRECTION('',(0.,0.,-1.));
#7954=DIRECTION('',(2.31296463463574E-16,-1.,0.));
#7955=DIRECTION('',(0.,0.,1.));
#7956=DIRECTION('center_axis',(0.,1.,0.));
#7957=DIRECTION('ref_axis',(0.,0.,1.));
#7958=DIRECTION('',(-1.,0.,0.));
#7959=DIRECTION('',(0.,0.,-1.));
#7960=DIRECTION('',(1.,0.,0.));
#7961=DIRECTION('',(0.,0.,1.));
#7962=DIRECTION('center_axis',(-1.,6.81286914308505E-17,0.));
#7963=DIRECTION('ref_axis',(-6.81286914308505E-17,-1.,0.));
#7964=DIRECTION('',(-6.81286914308505E-17,-1.,0.));
#7965=DIRECTION('',(0.,0.,-1.));
#7966=DIRECTION('',(6.81286914308505E-17,1.,0.));
#7967=DIRECTION('',(0.,0.,1.));
#7968=DIRECTION('center_axis',(0.,0.,1.));
#7969=DIRECTION('ref_axis',(1.,0.,0.));
#7970=DIRECTION('center_axis',(0.,0.,1.));
#7971=DIRECTION('ref_axis',(1.,0.,0.));
#7972=DIRECTION('center_axis',(0.,0.,1.));
#7973=DIRECTION('ref_axis',(1.,0.,0.));
#7974=DIRECTION('center_axis',(0.,0.,1.));
#7975=DIRECTION('ref_axis',(1.,0.,0.));
#7976=DIRECTION('',(-1.,-1.22464679914735E-16,0.));
#7977=DIRECTION('',(2.31296463463574E-16,-1.,0.));
#7978=DIRECTION('',(1.,0.,0.));
#7979=DIRECTION('',(6.81286914308505E-17,1.,0.));
#7980=DIRECTION('center_axis',(0.,0.,1.));
#7981=DIRECTION('ref_axis',(1.,0.,0.));
#7982=DIRECTION('center_axis',(0.,0.,-1.));
#7983=DIRECTION('ref_axis',(1.,0.,0.));
#7984=DIRECTION('center_axis',(0.,0.,-1.));
#7985=DIRECTION('ref_axis',(1.,0.,0.));
#7986=DIRECTION('center_axis',(0.,0.,-1.));
#7987=DIRECTION('ref_axis',(1.,5.33572772289561E-15,0.));
#7988=DIRECTION('',(-6.81286914308505E-17,-1.,0.));
#7989=DIRECTION('',(-1.,0.,0.));
#7990=DIRECTION('',(-2.31296463463574E-16,1.,0.));
#7991=DIRECTION('',(1.,1.22464679914735E-16,0.));
#7992=DIRECTION('center_axis',(1.,0.,0.));
#7993=DIRECTION('ref_axis',(0.,0.,-1.));
#7994=DIRECTION('',(0.,1.,0.));
#7995=DIRECTION('center_axis',(1.,0.,0.));
#7996=DIRECTION('ref_axis',(0.,0.,-1.));
#7997=DIRECTION('',(0.,0.,1.));
#7998=DIRECTION('',(0.,0.,-1.));
#7999=DIRECTION('',(0.,1.,0.));
#8000=DIRECTION('center_axis',(1.,2.7390370673318E-16,0.));
#8001=DIRECTION('ref_axis',(-2.7390370673318E-16,1.,0.));
#8002=DIRECTION('',(0.,0.,1.));
#8003=DIRECTION('center_axis',(-1.,-2.7390370673318E-16,0.));
#8004=DIRECTION('ref_axis',(-2.7390370673318E-16,1.,0.));
#8005=DIRECTION('',(-2.7390370673318E-16,1.,0.));
#8006=DIRECTION('',(-4.47852670343415E-16,-1.,0.));
#8007=DIRECTION('',(0.,0.,-1.));
#8008=DIRECTION('center_axis',(0.,-1.,0.));
#8009=DIRECTION('ref_axis',(0.,0.,-1.));
#8010=DIRECTION('',(-1.,0.,0.));
#8011=DIRECTION('center_axis',(0.,0.,1.));
#8012=DIRECTION('ref_axis',(1.,0.,0.));
#8013=DIRECTION('',(1.,0.,0.));
#8014=DIRECTION('center_axis',(1.,0.,0.));
#8015=DIRECTION('ref_axis',(0.,0.,-1.));
#8016=DIRECTION('center_axis',(0.,-1.,0.));
#8017=DIRECTION('ref_axis',(0.,0.,-1.));
#8018=DIRECTION('',(-1.,0.,0.));
#8019=DIRECTION('center_axis',(0.,0.,1.));
#8020=DIRECTION('ref_axis',(1.,0.,0.));
#8021=DIRECTION('center_axis',(1.,0.,0.));
#8022=DIRECTION('ref_axis',(0.,0.,-1.));
#8023=DIRECTION('center_axis',(-1.,0.,0.));
#8024=DIRECTION('ref_axis',(0.,0.,1.));
#8025=DIRECTION('center_axis',(1.,0.,0.));
#8026=DIRECTION('ref_axis',(0.,0.,-1.));
#8027=DIRECTION('center_axis',(1.,0.,-1.11022302462516E-16));
#8028=DIRECTION('ref_axis',(0.,-8.88178419700125E-16,-1.));
#8029=DIRECTION('center_axis',(0.,1.,0.));
#8030=DIRECTION('ref_axis',(-1.73472347597681E-15,0.,-1.));
#8031=DIRECTION('center_axis',(0.,0.,1.));
#8032=DIRECTION('ref_axis',(-1.,0.,0.));
#8033=DIRECTION('center_axis',(0.,1.,0.));
#8034=DIRECTION('ref_axis',(-1.,0.,0.));
#8035=DIRECTION('center_axis',(0.,0.,1.));
#8036=DIRECTION('ref_axis',(-1.,0.,0.));
#8037=DIRECTION('center_axis',(-1.73472347597681E-15,1.,0.));
#8038=DIRECTION('ref_axis',(1.,1.73472347597681E-15,0.));
#8039=DIRECTION('center_axis',(0.,0.,-1.));
#8040=DIRECTION('ref_axis',(-1.,0.,0.));
#8041=DIRECTION('center_axis',(0.,0.,1.));
#8042=DIRECTION('ref_axis',(1.,0.,0.));
#8043=DIRECTION('center_axis',(2.31296463463574E-16,-1.,0.));
#8044=DIRECTION('ref_axis',(1.,2.31296463463574E-16,0.));
#8045=DIRECTION('center_axis',(-2.16840434497101E-16,1.,0.));
#8046=DIRECTION('ref_axis',(-1.,-2.16840434497101E-16,0.));
#8047=DIRECTION('center_axis',(6.81286914308505E-17,1.,0.));
#8048=DIRECTION('ref_axis',(-1.,6.81286914308505E-17,0.));
#8049=DIRECTION('center_axis',(0.,0.,-1.));
#8050=DIRECTION('ref_axis',(-1.,0.,0.));
#8051=DIRECTION('center_axis',(0.,0.,1.));
#8052=DIRECTION('ref_axis',(1.,0.,0.));
#8053=DIRECTION('center_axis',(-1.,0.,0.));
#8054=DIRECTION('ref_axis',(0.,0.,1.));
#8055=DIRECTION('center_axis',(-1.,0.,-1.73472347597681E-15));
#8056=DIRECTION('ref_axis',(-1.73472347597681E-15,0.,1.));
#8057=DIRECTION('center_axis',(1.,0.,0.));
#8058=DIRECTION('ref_axis',(0.,0.,-1.));
#8059=DIRECTION('center_axis',(1.,0.,0.));
#8060=DIRECTION('ref_axis',(0.,0.,-1.));
#8061=DIRECTION('center_axis',(-1.73472347597681E-15,1.,0.));
#8062=DIRECTION('ref_axis',(1.,1.73472347597681E-15,0.));
#8063=DIRECTION('center_axis',(0.,1.,0.));
#8064=DIRECTION('ref_axis',(1.77635683940025E-15,0.,1.));
#8065=DIRECTION('center_axis',(1.,0.,0.));
#8066=DIRECTION('ref_axis',(0.,0.,1.));
#8067=DIRECTION('center_axis',(0.,0.,1.));
#8068=DIRECTION('ref_axis',(-1.,0.,0.));
#8069=DIRECTION('center_axis',(1.,0.,0.));
#8070=DIRECTION('ref_axis',(0.,0.,-1.));
#8071=DIRECTION('center_axis',(0.,1.,0.));
#8072=DIRECTION('ref_axis',(0.,0.,-1.));
#8073=DIRECTION('center_axis',(-2.31296463463574E-16,1.,0.));
#8074=DIRECTION('ref_axis',(-1.,-2.31296463463574E-16,0.));
#8075=DIRECTION('center_axis',(-2.16840434497101E-16,1.,6.50521303491302E-16));
#8076=DIRECTION('ref_axis',(-6.41463530422129E-47,-6.50521303491302E-16,
1.));
#8077=DIRECTION('center_axis',(0.,0.,-1.));
#8078=DIRECTION('ref_axis',(-1.,0.,0.));
#8079=DIRECTION('center_axis',(0.,0.,1.));
#8080=DIRECTION('ref_axis',(1.,0.,0.));
#8081=DIRECTION('center_axis',(-1.,-1.22464679914735E-16,0.));
#8082=DIRECTION('ref_axis',(1.22464679914735E-16,-1.,0.));
#8083=DIRECTION('center_axis',(1.,1.21972744404619E-16,0.));
#8084=DIRECTION('ref_axis',(-1.21972744404619E-16,1.,0.));
#8085=DIRECTION('center_axis',(0.,0.,1.));
#8086=DIRECTION('ref_axis',(-0.966517253196389,-0.25660163536834,0.));
#8087=DIRECTION('center_axis',(0.176867050811513,0.984234751640704,0.));
#8088=DIRECTION('ref_axis',(-0.984234751640704,0.176867050811512,0.));
#8089=DIRECTION('center_axis',(0.,0.,1.));
#8090=DIRECTION('ref_axis',(1.,0.,0.));
#8091=DIRECTION('center_axis',(-0.954169336796974,-0.299267232948117,8.79335597693182E-15));
#8092=DIRECTION('ref_axis',(0.299267232948117,-0.954169336796974,-6.57835715770868E-30));
#8093=DIRECTION('center_axis',(0.,0.,-1.));
#8094=DIRECTION('ref_axis',(-1.,0.,0.));
#8095=DIRECTION('center_axis',(0.,0.,1.));
#8096=DIRECTION('ref_axis',(1.,0.,0.));
#8097=DIRECTION('center_axis',(-6.81286914308505E-17,-1.,0.));
#8098=DIRECTION('ref_axis',(1.,-6.81286914308505E-17,0.));
#8099=DIRECTION('center_axis',(6.93889390390722E-15,1.,0.));
#8100=DIRECTION('ref_axis',(-1.,6.93889390390722E-15,0.));
#8101=DIRECTION('center_axis',(0.,0.,1.));
#8102=DIRECTION('ref_axis',(0.,-1.,0.));
#8103=DIRECTION('center_axis',(1.,-1.73472347597681E-15,0.));
#8104=DIRECTION('ref_axis',(-1.73472347597681E-15,-1.,0.));
#8105=DIRECTION('center_axis',(0.,0.,1.));
#8106=DIRECTION('ref_axis',(1.,0.,0.));
#8107=DIRECTION('center_axis',(0.,0.,-1.));
#8108=DIRECTION('ref_axis',(1.,0.,0.));
#8109=DIRECTION('center_axis',(-1.11022302462516E-16,1.,0.));
#8110=DIRECTION('ref_axis',(-1.,0.,8.88178419700125E-16));
#8111=DIRECTION('center_axis',(0.,0.,1.));
#8112=DIRECTION('ref_axis',(-1.,0.,0.));
#8113=DIRECTION('center_axis',(1.,0.,0.));
#8114=DIRECTION('ref_axis',(0.,-1.,7.105427357601E-15));
#8115=DIRECTION('center_axis',(-0.992279004699137,-0.124025710372042,0.));
#8116=DIRECTION('ref_axis',(-0.124025710372042,0.992279004699137,0.));
#8117=DIRECTION('center_axis',(1.,1.22464679914735E-16,0.));
#8118=DIRECTION('ref_axis',(-1.22464679914735E-16,1.,0.));
#8119=DIRECTION('center_axis',(1.,1.21972744404619E-16,7.93458686805043E-32));
#8120=DIRECTION('ref_axis',(-1.21972744404619E-16,1.,1.69964635189105E-63));
#8121=DIRECTION('center_axis',(0.,0.,-1.));
#8122=DIRECTION('ref_axis',(-1.,0.,0.));
#8123=DIRECTION('center_axis',(0.,0.,-1.));
#8124=DIRECTION('ref_axis',(1.,0.,0.));
#8125=DIRECTION('center_axis',(0.,0.,-1.));
#8126=DIRECTION('ref_axis',(-1.,0.,0.));
#8127=DIRECTION('center_axis',(0.,0.,1.));
#8128=DIRECTION('ref_axis',(1.,0.,0.));
#8129=DIRECTION('center_axis',(0.,0.,1.));
#8130=DIRECTION('ref_axis',(1.,0.,0.));
#8131=DIRECTION('center_axis',(-0.954169336796977,-0.299267232948109,0.));
#8132=DIRECTION('ref_axis',(0.299267232948109,-0.954169336796977,0.));
#8133=DIRECTION('center_axis',(0.,0.,1.));
#8134=DIRECTION('ref_axis',(1.,0.,0.));
#8135=DIRECTION('center_axis',(1.11022302462516E-16,1.,0.));
#8136=DIRECTION('ref_axis',(1.,0.,0.));
#8137=DIRECTION('center_axis',(-0.176867050811505,-0.984234751640705,-7.65406697331636E-15));
#8138=DIRECTION('ref_axis',(-0.984234751640705,0.176867050811505,4.00542835088251E-31));
#8139=DIRECTION('center_axis',(0.,0.,1.));
#8140=DIRECTION('ref_axis',(-0.966517253196389,-0.25660163536834,0.));
#8141=DIRECTION('center_axis',(0.0933963198450884,0.961399932042651,0.25881904510252));
#8142=DIRECTION('ref_axis',(2.68671235148266E-18,-0.259955306903251,0.965620649330179));
#8143=DIRECTION('',(0.0933963198450884,0.961399932042651,0.25881904510252));
#8144=DIRECTION('',(0.0933963198450884,0.961399932042651,0.25881904510252));
#8145=DIRECTION('center_axis',(-0.386759736903912,-0.204506906446147,0.899218455730221));
#8146=DIRECTION('ref_axis',(0.918633667079783,1.12376124846612E-18,0.395110346242099));
#8147=DIRECTION('',(0.0933963198450936,0.96139993204265,0.258819045102522));
#8148=DIRECTION('center_axis',(-0.346541138612831,0.275090808425737,-0.896791105201539));
#8149=DIRECTION('ref_axis',(-0.932779367662293,-3.90319787005602E-18,0.360447848188239));
#8150=DIRECTION('',(-0.0933963198450826,-0.961399932042651,-0.258819045102522));
#8151=DIRECTION('center_axis',(0.0933963198450826,0.961399932042651,0.258819045102522));
#8152=DIRECTION('ref_axis',(-0.163713918954279,0.271246303466574,-0.948484683901828));
#8153=DIRECTION('center_axis',(0.0933963198450936,0.96139993204265,0.258819045102522));
#8154=DIRECTION('ref_axis',(4.28128594136413E-18,-0.259955306903254,0.965620649330178));
#8155=DIRECTION('axis',(0.,0.,1.));
#8156=DIRECTION('refdir',(1.,0.,0.));
#8157=DIRECTION('axis',(0.,0.,1.));
#8158=DIRECTION('refdir',(1.,0.,0.));
#8159=DIRECTION('center_axis',(0.,0.,1.));
#8160=DIRECTION('ref_axis',(1.,0.,0.));
#8161=DIRECTION('center_axis',(0.707106781186558,-5.01171544695272E-14,
0.707106781186537));
#8162=DIRECTION('ref_axis',(0.707106781186537,1.30563837326012E-11,-0.707106781186558));
#8163=DIRECTION('',(0.,0.,1.));
#8164=DIRECTION('center_axis',(-0.707106781186548,-3.66800410274155E-14,
0.707106781186547));
#8165=DIRECTION('ref_axis',(0.707106781186547,-1.32695584283249E-13,0.707106781186548));
#8166=DIRECTION('',(0.,0.,1.));
#8167=DIRECTION('center_axis',(0.707106781186548,-2.49447284670762E-16,
-0.707106781186547));
#8168=DIRECTION('ref_axis',(0.707106781186547,3.43199962798826E-15,0.707106781186548));
#8169=DIRECTION('',(0.,0.,1.));
#8170=DIRECTION('center_axis',(-0.707106781186548,-5.83546107254331E-15,
0.707106781186547));
#8171=DIRECTION('ref_axis',(0.707106781186547,-8.39541658988548E-14,0.707106781186548));
#8172=DIRECTION('',(0.,0.,-1.));
#8173=DIRECTION('center_axis',(0.70710678118654,-3.75878658521447E-14,0.707106781186555));
#8174=DIRECTION('ref_axis',(0.707106781186555,-7.50458522379288E-12,-0.70710678118654));
#8175=DIRECTION('center_axis',(0.,-1.,0.));
#8176=DIRECTION('ref_axis',(0.,0.,-1.));
#8177=DIRECTION('center_axis',(0.,1.,0.));
#8178=DIRECTION('ref_axis',(0.,0.,1.));
#8179=DIRECTION('',(0.,-1.,0.));
#8180=DIRECTION('center_axis',(0.,-1.,0.));
#8181=DIRECTION('ref_axis',(0.,0.,-1.));
#8182=DIRECTION('center_axis',(0.,1.,0.));
#8183=DIRECTION('ref_axis',(0.,0.,1.));
#8184=DIRECTION('center_axis',(0.,-1.,0.));
#8185=DIRECTION('ref_axis',(0.,0.,-1.));
#8186=DIRECTION('',(0.,-1.,0.));
#8187=DIRECTION('center_axis',(0.,1.,0.));
#8188=DIRECTION('ref_axis',(0.,0.,-1.));
#8189=DIRECTION('center_axis',(0.,1.,0.));
#8190=DIRECTION('ref_axis',(0.,0.,1.));
#8191=DIRECTION('center_axis',(0.,-1.,0.));
#8192=DIRECTION('ref_axis',(0.,0.,1.));
#8193=DIRECTION('',(0.,-1.,0.));
#8194=DIRECTION('center_axis',(0.,-1.,0.));
#8195=DIRECTION('ref_axis',(0.,0.,-1.));
#8196=DIRECTION('center_axis',(0.,1.,0.));
#8197=DIRECTION('ref_axis',(0.,0.,1.));
#8198=DIRECTION('center_axis',(0.,-1.,0.));
#8199=DIRECTION('ref_axis',(0.,0.,1.));
#8200=DIRECTION('',(0.,-1.,0.));
#8201=DIRECTION('center_axis',(0.,1.,0.));
#8202=DIRECTION('ref_axis',(0.,0.,-1.));
#8203=DIRECTION('center_axis',(0.,-1.,0.));
#8204=DIRECTION('ref_axis',(0.,0.,-1.));
#8205=DIRECTION('center_axis',(0.,-1.,-1.24352412568707E-16));
#8206=DIRECTION('ref_axis',(0.,-1.24352412568707E-16,1.));
#8207=DIRECTION('',(0.,-1.,0.));
#8208=DIRECTION('center_axis',(0.,-1.,0.));
#8209=DIRECTION('ref_axis',(0.,0.,-1.));
#8210=DIRECTION('',(0.,-1.,0.));
#8211=DIRECTION('center_axis',(0.,1.,1.24352412568707E-16));
#8212=DIRECTION('ref_axis',(0.,1.24352412568707E-16,-1.));
#8213=DIRECTION('center_axis',(0.,0.,-1.));
#8214=DIRECTION('ref_axis',(1.,0.,0.));
#8215=DIRECTION('center_axis',(0.,1.15648231731787E-16,-1.));
#8216=DIRECTION('ref_axis',(0.,1.,1.15648231731787E-16));
#8217=DIRECTION('center_axis',(0.,0.,1.));
#8218=DIRECTION('ref_axis',(-1.,0.,0.));
#8219=DIRECTION('',(0.0174524064372835,-2.1373033680838E-18,0.999847695156391));
#8220=DIRECTION('center_axis',(0.,0.,1.));
#8221=DIRECTION('ref_axis',(-1.,0.,0.));
#8222=DIRECTION('center_axis',(0.707106781186548,0.,0.707106781186548));
#8223=DIRECTION('ref_axis',(0.707106781186548,0.,-0.707106781186548));
#8224=DIRECTION('',(-0.707106781186547,0.,0.707106781186547));
#8225=DIRECTION('',(0.,-1.,0.));
#8226=DIRECTION('center_axis',(0.,-1.,0.));
#8227=DIRECTION('ref_axis',(0.,0.,-1.));
#8228=DIRECTION('',(0.707106781186548,0.,0.707106781186548));
#8229=DIRECTION('center_axis',(0.,-1.,0.));
#8230=DIRECTION('ref_axis',(0.,0.,-1.));
#8231=DIRECTION('center_axis',(0.,1.,0.));
#8232=DIRECTION('ref_axis',(0.,0.,1.));
#8233=DIRECTION('',(-0.707106781186547,0.,0.707106781186547));
#8234=DIRECTION('',(-0.707106781186548,0.,-0.707106781186548));
#8235=DIRECTION('center_axis',(0.,1.,0.));
#8236=DIRECTION('ref_axis',(0.,0.,1.));
#8237=DIRECTION('center_axis',(-0.707106781186547,0.,-0.707106781186548));
#8238=DIRECTION('ref_axis',(-0.707106781186548,0.,0.707106781186547));
#8239=DIRECTION('',(-0.707106781186548,0.,0.707106781186547));
#8240=DIRECTION('',(0.,1.,0.));
#8241=DIRECTION('',(-0.707106781186548,0.,0.707106781186547));
#8242=DIRECTION('',(0.,-1.,0.));
#8243=DIRECTION('center_axis',(0.,0.,-1.));
#8244=DIRECTION('ref_axis',(-1.,-1.22464679914735E-16,0.));
#8245=DIRECTION('center_axis',(0.,0.,-1.));
#8246=DIRECTION('ref_axis',(1.,1.77635683940025E-15,0.));
#8247=DIRECTION('center_axis',(0.,-1.,0.));
#8248=DIRECTION('ref_axis',(-0.185273532463833,0.,0.982686988907644));
#8249=DIRECTION('',(0.,1.,0.));
#8250=DIRECTION('center_axis',(0.,1.,1.24352412568707E-16));
#8251=DIRECTION('ref_axis',(0.,-1.24352412568707E-16,1.));
#8252=DIRECTION('center_axis',(0.,-1.,-1.24352412568707E-16));
#8253=DIRECTION('ref_axis',(0.,1.24352412568707E-16,-1.));
#8254=DIRECTION('center_axis',(0.,-1.,0.));
#8255=DIRECTION('ref_axis',(3.0760962761356E-5,0.,0.999999999526882));
#8256=DIRECTION('',(0.,1.,0.));
#8257=DIRECTION('center_axis',(0.,1.,0.));
#8258=DIRECTION('ref_axis',(0.,0.,-1.));
#8259=DIRECTION('',(0.,-1.,0.));
#8260=DIRECTION('center_axis',(0.,-1.,0.));
#8261=DIRECTION('ref_axis',(0.,0.,1.));
#8262=DIRECTION('center_axis',(0.,1.15648231731787E-16,-1.));
#8263=DIRECTION('ref_axis',(0.,1.,1.15648231731787E-16));
#8264=DIRECTION('',(-1.,0.,0.));
#8265=DIRECTION('',(0.,-1.,-1.15648231731787E-16));
#8266=DIRECTION('',(-1.,0.,0.));
#8267=DIRECTION('center_axis',(0.,1.,1.24352412568707E-16));
#8268=DIRECTION('ref_axis',(0.,-1.24352412568707E-16,1.));
#8269=DIRECTION('',(0.,1.24352412568707E-16,-1.));
#8270=DIRECTION('center_axis',(0.,-1.,-1.24352412568707E-16));
#8271=DIRECTION('ref_axis',(0.,1.24352412568707E-16,-1.));
#8272=DIRECTION('',(0.,-1.24352412568707E-16,1.));
#8273=DIRECTION('center_axis',(-1.,0.,0.));
#8274=DIRECTION('ref_axis',(0.,0.,1.));
#8275=DIRECTION('center_axis',(0.,0.,1.));
#8276=DIRECTION('ref_axis',(1.,0.,0.));
#8277=DIRECTION('',(-1.,0.,0.));
#8278=DIRECTION('',(0.,1.,0.));
#8279=DIRECTION('',(-1.,0.,0.));
#8280=DIRECTION('center_axis',(0.,-1.,0.));
#8281=DIRECTION('ref_axis',(0.,0.,-1.));
#8282=DIRECTION('',(0.707106781186548,0.,-0.707106781186547));
#8283=DIRECTION('center_axis',(0.,1.,0.));
#8284=DIRECTION('ref_axis',(0.,0.,-1.));
#8285=DIRECTION('',(0.707106781186548,0.,0.707106781186548));
#8286=DIRECTION('',(-1.,0.,0.));
#8287=DIRECTION('',(0.707106781186548,0.,0.707106781186548));
#8288=DIRECTION('center_axis',(0.,1.,0.));
#8289=DIRECTION('ref_axis',(-3.46944695195361E-15,0.,-1.));
#8290=DIRECTION('center_axis',(0.,0.,-1.));
#8291=DIRECTION('ref_axis',(-1.,0.,0.));
#8292=DIRECTION('',(0.,-1.,0.));
#8293=DIRECTION('',(-1.,0.,0.));
#8294=DIRECTION('center_axis',(0.,1.,0.));
#8295=DIRECTION('ref_axis',(0.,0.,1.));
#8296=DIRECTION('',(0.707106781186548,0.,0.707106781186548));
#8297=DIRECTION('center_axis',(0.,-1.,0.));
#8298=DIRECTION('ref_axis',(3.46944695195361E-15,0.,1.));
#8299=DIRECTION('center_axis',(0.,-1.,0.));
#8300=DIRECTION('ref_axis',(-3.46944695195361E-15,0.,1.));
#8301=DIRECTION('',(0.707106781186548,0.,0.707106781186548));
#8302=DIRECTION('center_axis',(-0.707106781186548,0.,0.707106781186547));
#8303=DIRECTION('ref_axis',(0.707106781186547,0.,0.707106781186548));
#8304=DIRECTION('',(-0.707106781186548,0.,-0.707106781186548));
#8305=DIRECTION('',(0.,1.,0.));
#8306=DIRECTION('',(0.,1.,0.));
#8307=DIRECTION('',(0.707106781186548,0.,0.707106781186548));
#8308=DIRECTION('',(0.,1.,0.));
#8309=DIRECTION('center_axis',(0.707106781186548,0.,-0.707106781186547));
#8310=DIRECTION('ref_axis',(-0.707106781186547,0.,-0.707106781186548));
#8311=DIRECTION('',(-0.707106781186548,0.,-0.707106781186548));
#8312=DIRECTION('',(0.707106781186548,0.,0.707106781186548));
#8313=DIRECTION('',(0.,-1.,0.));
#8314=DIRECTION('',(0.,-1.,0.));
#8315=DIRECTION('center_axis',(-0.707106781186547,0.,-0.707106781186548));
#8316=DIRECTION('ref_axis',(-0.707106781186548,0.,0.707106781186547));
#8317=DIRECTION('',(0.707106781186548,0.,-0.707106781186547));
#8318=DIRECTION('',(0.,1.,0.));
#8319=DIRECTION('',(0.,-1.,0.));
#8320=DIRECTION('center_axis',(0.707106781186548,0.,0.707106781186548));
#8321=DIRECTION('ref_axis',(0.707106781186548,0.,-0.707106781186548));
#8322=DIRECTION('',(0.,-1.,0.));
#8323=DIRECTION('center_axis',(0.,-1.,0.));
#8324=DIRECTION('ref_axis',(0.,0.,-1.));
#8325=DIRECTION('center_axis',(0.,1.,0.));
#8326=DIRECTION('ref_axis',(-3.46944695195361E-15,0.,-1.));
#8327=DIRECTION('center_axis',(0.,1.,0.));
#8328=DIRECTION('ref_axis',(0.,0.,-1.));
#8329=DIRECTION('center_axis',(0.,1.,0.));
#8330=DIRECTION('ref_axis',(0.,0.,1.));
#8331=DIRECTION('center_axis',(0.,-1.,0.));
#8332=DIRECTION('ref_axis',(0.,0.,1.));
#8333=DIRECTION('center_axis',(0.,-1.,0.));
#8334=DIRECTION('ref_axis',(-3.46944695195361E-15,0.,1.));
#8335=DIRECTION('center_axis',(0.,-1.,0.));
#8336=DIRECTION('ref_axis',(0.,0.,-1.));
#8337=DIRECTION('center_axis',(0.,-1.,0.));
#8338=DIRECTION('ref_axis',(0.,0.,-1.));
#8339=DIRECTION('center_axis',(0.,-1.,0.));
#8340=DIRECTION('ref_axis',(0.,0.,-1.));
#8341=DIRECTION('center_axis',(0.,-1.,0.));
#8342=DIRECTION('ref_axis',(0.,0.,-1.));
#8343=DIRECTION('center_axis',(0.,1.,0.));
#8344=DIRECTION('ref_axis',(1.45473230946492E-15,0.,-1.));
#8345=DIRECTION('center_axis',(0.,1.,0.));
#8346=DIRECTION('ref_axis',(1.45473230946492E-15,0.,-1.));
#8347=DIRECTION('center_axis',(0.,1.,0.));
#8348=DIRECTION('ref_axis',(-1.22464679914735E-16,0.,-1.));
#8349=DIRECTION('center_axis',(0.,0.,-1.));
#8350=DIRECTION('ref_axis',(-1.,0.,0.));
#8351=DIRECTION('',(1.,0.,0.));
#8352=DIRECTION('',(0.,1.,0.));
#8353=DIRECTION('',(-1.,0.,0.));
#8354=DIRECTION('',(0.,-1.,0.));
#8355=DIRECTION('center_axis',(0.,-1.,0.));
#8356=DIRECTION('ref_axis',(0.,0.,-1.));
#8357=DIRECTION('',(0.,0.,1.));
#8358=DIRECTION('center_axis',(0.,-1.,0.));
#8359=DIRECTION('ref_axis',(0.,0.,-1.));
#8360=DIRECTION('center_axis',(0.,-1.,0.));
#8361=DIRECTION('ref_axis',(0.,0.,-1.));
#8362=DIRECTION('',(0.,0.,1.));
#8363=DIRECTION('center_axis',(1.,0.,0.));
#8364=DIRECTION('ref_axis',(0.,0.,-1.));
#8365=DIRECTION('',(0.,0.,1.));
#8366=DIRECTION('',(0.,-1.,0.));
#8367=DIRECTION('center_axis',(0.,1.,0.));
#8368=DIRECTION('ref_axis',(0.,0.,1.));
#8369=DIRECTION('center_axis',(0.,1.,0.));
#8370=DIRECTION('ref_axis',(0.,0.,1.));
#8371=DIRECTION('',(0.,0.,1.));
#8372=DIRECTION('center_axis',(0.,1.,0.));
#8373=DIRECTION('ref_axis',(0.,0.,1.));
#8374=DIRECTION('center_axis',(-1.,0.,0.));
#8375=DIRECTION('ref_axis',(0.,0.,1.));
#8376=DIRECTION('',(0.,1.,0.));
#8377=DIRECTION('center_axis',(0.,-1.,0.));
#8378=DIRECTION('ref_axis',(0.,0.,-1.));
#8379=DIRECTION('center_axis',(0.,1.,0.));
#8380=DIRECTION('ref_axis',(0.,0.,1.));
#8381=DIRECTION('axis',(0.,0.,1.));
#8382=DIRECTION('refdir',(1.,0.,0.));
#8383=DIRECTION('center_axis',(0.,-1.,0.));
#8384=DIRECTION('ref_axis',(0.,0.,-1.));
#8385=DIRECTION('center_axis',(0.,1.,0.));
#8386=DIRECTION('ref_axis',(0.,0.,1.));
#8387=DIRECTION('',(0.,-1.,0.));
#8388=DIRECTION('center_axis',(0.,-1.,0.));
#8389=DIRECTION('ref_axis',(0.,0.,-1.));
#8390=DIRECTION('center_axis',(0.,1.,0.));
#8391=DIRECTION('ref_axis',(0.,0.,1.));
#8392=DIRECTION('center_axis',(0.,-1.,0.));
#8393=DIRECTION('ref_axis',(0.,0.,-1.));
#8394=DIRECTION('',(0.,-1.,0.));
#8395=DIRECTION('center_axis',(0.,1.,0.));
#8396=DIRECTION('ref_axis',(0.,0.,-1.));
#8397=DIRECTION('center_axis',(0.,1.,0.));
#8398=DIRECTION('ref_axis',(0.,0.,1.));
#8399=DIRECTION('center_axis',(0.,-1.,0.));
#8400=DIRECTION('ref_axis',(0.,0.,1.));
#8401=DIRECTION('',(0.,-1.,0.));
#8402=DIRECTION('center_axis',(0.,-1.,0.));
#8403=DIRECTION('ref_axis',(0.,0.,-1.));
#8404=DIRECTION('center_axis',(0.,1.,0.));
#8405=DIRECTION('ref_axis',(0.,0.,1.));
#8406=DIRECTION('center_axis',(0.,-1.,0.));
#8407=DIRECTION('ref_axis',(0.,0.,1.));
#8408=DIRECTION('',(0.,-1.,0.));
#8409=DIRECTION('center_axis',(0.,1.,0.));
#8410=DIRECTION('ref_axis',(0.,0.,-1.));
#8411=DIRECTION('center_axis',(0.,-1.,0.));
#8412=DIRECTION('ref_axis',(0.,0.,-1.));
#8413=DIRECTION('center_axis',(0.,-1.,-1.24352412568707E-16));
#8414=DIRECTION('ref_axis',(0.,-1.24352412568707E-16,1.));
#8415=DIRECTION('',(0.,-1.,0.));
#8416=DIRECTION('center_axis',(0.,-1.,0.));
#8417=DIRECTION('ref_axis',(0.,0.,-1.));
#8418=DIRECTION('',(0.,-1.,0.));
#8419=DIRECTION('center_axis',(0.,1.,1.24352412568707E-16));
#8420=DIRECTION('ref_axis',(0.,1.24352412568707E-16,-1.));
#8421=DIRECTION('center_axis',(0.,0.,-1.));
#8422=DIRECTION('ref_axis',(1.,0.,0.));
#8423=DIRECTION('center_axis',(0.,0.,1.));
#8424=DIRECTION('ref_axis',(-1.,1.77635684682688E-15,0.));
#8425=DIRECTION('center_axis',(0.,0.,1.));
#8426=DIRECTION('ref_axis',(-1.,0.,0.));
#8427=DIRECTION('',(0.0174524064372835,-2.1373033680838E-18,0.999847695156391));
#8428=DIRECTION('center_axis',(0.,0.,1.));
#8429=DIRECTION('ref_axis',(-1.,0.,0.));
#8430=DIRECTION('center_axis',(0.,-1.,0.));
#8431=DIRECTION('ref_axis',(0.,0.,-1.));
#8432=DIRECTION('center_axis',(0.,1.,1.24352412568707E-16));
#8433=DIRECTION('ref_axis',(0.,-1.24352412568707E-16,1.));
#8434=DIRECTION('',(0.,-1.,0.));
#8435=DIRECTION('',(0.,-1.,0.));
#8436=DIRECTION('center_axis',(0.,-1.,-1.24352412568707E-16));
#8437=DIRECTION('ref_axis',(0.,1.24352412568707E-16,-1.));
#8438=DIRECTION('',(0.,1.,0.));
#8439=DIRECTION('center_axis',(-0.707106781186547,0.,-0.707106781186548));
#8440=DIRECTION('ref_axis',(-0.707106781186548,0.,0.707106781186547));
#8441=DIRECTION('',(-0.707106781186548,0.,0.707106781186547));
#8442=DIRECTION('',(0.,1.,0.));
#8443=DIRECTION('',(-0.707106781186548,0.,0.707106781186547));
#8444=DIRECTION('',(0.,-1.,0.));
#8445=DIRECTION('center_axis',(0.,0.,-1.));
#8446=DIRECTION('ref_axis',(-1.,-1.22464679914735E-16,0.));
#8447=DIRECTION('center_axis',(0.,0.,-1.));
#8448=DIRECTION('ref_axis',(1.,1.77635684759209E-15,0.));
#8449=DIRECTION('center_axis',(0.,-1.,0.));
#8450=DIRECTION('ref_axis',(3.0760962761356E-5,0.,0.999999999526882));
#8451=DIRECTION('',(0.,1.,0.));
#8452=DIRECTION('center_axis',(0.,1.,0.));
#8453=DIRECTION('ref_axis',(0.,0.,-1.));
#8454=DIRECTION('',(0.,-1.,0.));
#8455=DIRECTION('center_axis',(0.,-1.,0.));
#8456=DIRECTION('ref_axis',(0.,0.,1.));
#8457=DIRECTION('center_axis',(0.,1.15648231731787E-16,-1.));
#8458=DIRECTION('ref_axis',(0.,1.,1.15648231731787E-16));
#8459=DIRECTION('center_axis',(0.,1.15648231731787E-16,-1.));
#8460=DIRECTION('ref_axis',(0.,1.,1.15648231731787E-16));
#8461=DIRECTION('',(-1.,0.,0.));
#8462=DIRECTION('',(0.,-1.,-1.15648231731787E-16));
#8463=DIRECTION('',(-1.,0.,0.));
#8464=DIRECTION('center_axis',(0.,1.,1.24352412568707E-16));
#8465=DIRECTION('ref_axis',(0.,-1.24352412568707E-16,1.));
#8466=DIRECTION('center_axis',(0.,-1.,-1.24352412568707E-16));
#8467=DIRECTION('ref_axis',(0.,-1.24352412568707E-16,1.));
#8468=DIRECTION('center_axis',(0.,1.,1.24352412568707E-16));
#8469=DIRECTION('ref_axis',(0.,-1.24352412568707E-16,1.));
#8470=DIRECTION('',(0.,1.24352412568707E-16,-1.));
#8471=DIRECTION('center_axis',(0.,-1.,-1.24352412568707E-16));
#8472=DIRECTION('ref_axis',(0.,1.24352412568707E-16,-1.));
#8473=DIRECTION('center_axis',(0.,-1.,-1.24352412568707E-16));
#8474=DIRECTION('ref_axis',(0.,1.24352412568707E-16,-1.));
#8475=DIRECTION('center_axis',(0.,1.,1.24352412568707E-16));
#8476=DIRECTION('ref_axis',(0.,1.24352412568707E-16,-1.));
#8477=DIRECTION('',(0.,-1.24352412568707E-16,1.));
#8478=DIRECTION('center_axis',(-1.,0.,0.));
#8479=DIRECTION('ref_axis',(0.,0.,1.));
#8480=DIRECTION('center_axis',(0.,0.,1.));
#8481=DIRECTION('ref_axis',(1.,0.,0.));
#8482=DIRECTION('',(-1.,0.,0.));
#8483=DIRECTION('',(0.,1.,0.));
#8484=DIRECTION('',(-1.,0.,0.));
#8485=DIRECTION('center_axis',(0.,-1.,0.));
#8486=DIRECTION('ref_axis',(0.,0.,-1.));
#8487=DIRECTION('',(0.707106781186548,0.,-0.707106781186547));
#8488=DIRECTION('center_axis',(0.,1.,0.));
#8489=DIRECTION('ref_axis',(0.,0.,-1.));
#8490=DIRECTION('',(0.707106781186548,0.,0.707106781186548));
#8491=DIRECTION('',(-1.,0.,0.));
#8492=DIRECTION('',(0.707106781186548,0.,0.707106781186548));
#8493=DIRECTION('center_axis',(0.,1.,0.));
#8494=DIRECTION('ref_axis',(-7.70988211545247E-15,0.,-1.));
#8495=DIRECTION('center_axis',(0.,0.,-1.));
#8496=DIRECTION('ref_axis',(-1.,0.,0.));
#8497=DIRECTION('',(0.,-1.,0.));
#8498=DIRECTION('',(-1.,0.,0.));
#8499=DIRECTION('center_axis',(0.,1.,0.));
#8500=DIRECTION('ref_axis',(0.,0.,1.));
#8501=DIRECTION('',(0.707106781186548,0.,0.707106781186548));
#8502=DIRECTION('center_axis',(0.,-1.,0.));
#8503=DIRECTION('ref_axis',(-3.85494105772624E-15,0.,1.));
#8504=DIRECTION('center_axis',(0.,-1.,0.));
#8505=DIRECTION('ref_axis',(3.85494105772624E-15,0.,1.));
#8506=DIRECTION('',(0.707106781186548,0.,0.707106781186548));
#8507=DIRECTION('center_axis',(-0.707106781186548,0.,0.707106781186547));
#8508=DIRECTION('ref_axis',(0.707106781186547,0.,0.707106781186548));
#8509=DIRECTION('',(0.,1.,0.));
#8510=DIRECTION('',(0.707106781186547,0.,0.707106781186548));
#8511=DIRECTION('',(0.,1.,0.));
#8512=DIRECTION('',(-0.707106781186547,0.,-0.707106781186548));
#8513=DIRECTION('',(0.,1.,0.));
#8514=DIRECTION('center_axis',(0.707106781186548,0.,-0.707106781186547));
#8515=DIRECTION('ref_axis',(-0.707106781186547,0.,-0.707106781186548));
#8516=DIRECTION('',(-0.707106781186547,0.,-0.707106781186548));
#8517=DIRECTION('',(0.,-1.,0.));
#8518=DIRECTION('',(0.707106781186547,0.,0.707106781186548));
#8519=DIRECTION('',(0.,-1.,0.));
#8520=DIRECTION('',(0.,-1.,0.));
#8521=DIRECTION('center_axis',(-0.707106781186547,0.,-0.707106781186548));
#8522=DIRECTION('ref_axis',(-0.707106781186548,0.,0.707106781186547));
#8523=DIRECTION('',(0.707106781186548,0.,-0.707106781186547));
#8524=DIRECTION('',(0.,1.,0.));
#8525=DIRECTION('',(0.,-1.,0.));
#8526=DIRECTION('center_axis',(0.707106781186548,0.,0.707106781186548));
#8527=DIRECTION('ref_axis',(0.707106781186548,0.,-0.707106781186548));
#8528=DIRECTION('',(-0.707106781186547,0.,0.707106781186547));
#8529=DIRECTION('',(0.,1.,0.));
#8530=DIRECTION('',(-0.707106781186547,0.,0.707106781186547));
#8531=DIRECTION('',(0.,-1.,0.));
#8532=DIRECTION('center_axis',(0.,-1.,0.));
#8533=DIRECTION('ref_axis',(0.,0.,-1.));
#8534=DIRECTION('center_axis',(0.,1.,0.));
#8535=DIRECTION('ref_axis',(0.,0.,-1.));
#8536=DIRECTION('center_axis',(0.,-1.,0.));
#8537=DIRECTION('ref_axis',(0.,0.,-1.));
#8538=DIRECTION('center_axis',(0.,-1.,0.));
#8539=DIRECTION('ref_axis',(0.,0.,-1.));
#8540=DIRECTION('center_axis',(0.,1.,0.));
#8541=DIRECTION('ref_axis',(-7.70988211545247E-15,0.,-1.));
#8542=DIRECTION('center_axis',(0.,1.,0.));
#8543=DIRECTION('ref_axis',(0.,0.,1.));
#8544=DIRECTION('center_axis',(0.,-1.,0.));
#8545=DIRECTION('ref_axis',(3.85494105772624E-15,0.,1.));
#8546=DIRECTION('center_axis',(0.,-1.,0.));
#8547=DIRECTION('ref_axis',(3.85494105772624E-15,0.,1.));
#8548=DIRECTION('center_axis',(0.,1.,0.));
#8549=DIRECTION('ref_axis',(0.,0.,1.));
#8550=DIRECTION('center_axis',(0.,1.,0.));
#8551=DIRECTION('ref_axis',(0.,0.,1.));
#8552=DIRECTION('center_axis',(0.,-1.,0.));
#8553=DIRECTION('ref_axis',(0.,0.,-1.));
#8554=DIRECTION('center_axis',(0.,-1.,0.));
#8555=DIRECTION('ref_axis',(0.,0.,-1.));
#8556=DIRECTION('center_axis',(0.,1.,0.));
#8557=DIRECTION('ref_axis',(0.,0.,1.));
#8558=DIRECTION('center_axis',(0.,-1.,0.));
#8559=DIRECTION('ref_axis',(0.,0.,-1.));
#8560=DIRECTION('center_axis',(0.,-1.,0.));
#8561=DIRECTION('ref_axis',(0.,0.,-1.));
#8562=DIRECTION('center_axis',(0.,1.,0.));
#8563=DIRECTION('ref_axis',(1.22464679914735E-16,0.,-1.));
#8564=DIRECTION('center_axis',(0.,1.,0.));
#8565=DIRECTION('ref_axis',(1.22464679914735E-16,0.,-1.));
#8566=DIRECTION('center_axis',(0.,1.,0.));
#8567=DIRECTION('ref_axis',(1.01064309961486E-15,0.,-1.));
#8568=DIRECTION('center_axis',(0.,0.,-1.));
#8569=DIRECTION('ref_axis',(-1.,0.,0.));
#8570=DIRECTION('',(1.,0.,0.));
#8571=DIRECTION('',(0.,1.,0.));
#8572=DIRECTION('',(-1.,0.,0.));
#8573=DIRECTION('',(0.,-1.,0.));
#8574=DIRECTION('center_axis',(0.,-1.,0.));
#8575=DIRECTION('ref_axis',(0.,0.,-1.));
#8576=DIRECTION('',(0.,0.,1.));
#8577=DIRECTION('center_axis',(0.,-1.,0.));
#8578=DIRECTION('ref_axis',(0.,0.,-1.));
#8579=DIRECTION('center_axis',(0.,-1.,0.));
#8580=DIRECTION('ref_axis',(0.,0.,-1.));
#8581=DIRECTION('',(0.,0.,1.));
#8582=DIRECTION('center_axis',(1.,0.,0.));
#8583=DIRECTION('ref_axis',(0.,0.,-1.));
#8584=DIRECTION('',(0.,0.,1.));
#8585=DIRECTION('',(0.,-1.,0.));
#8586=DIRECTION('center_axis',(0.,1.,0.));
#8587=DIRECTION('ref_axis',(0.,0.,1.));
#8588=DIRECTION('center_axis',(0.,1.,0.));
#8589=DIRECTION('ref_axis',(0.,0.,1.));
#8590=DIRECTION('',(0.,0.,1.));
#8591=DIRECTION('center_axis',(0.,1.,0.));
#8592=DIRECTION('ref_axis',(0.,0.,1.));
#8593=DIRECTION('center_axis',(-1.,0.,0.));
#8594=DIRECTION('ref_axis',(0.,0.,1.));
#8595=DIRECTION('',(0.,1.,0.));
#8596=DIRECTION('center_axis',(0.,-1.,0.));
#8597=DIRECTION('ref_axis',(0.,0.,-1.));
#8598=DIRECTION('center_axis',(0.,1.,0.));
#8599=DIRECTION('ref_axis',(0.,0.,1.));
#8600=DIRECTION('center_axis',(0.,-1.,0.));
#8601=DIRECTION('ref_axis',(0.,0.,-1.));
#8602=DIRECTION('',(0.,1.,0.));
#8603=DIRECTION('center_axis',(0.,-1.,0.));
#8604=DIRECTION('ref_axis',(0.,0.,-1.));
#8605=DIRECTION('',(0.,1.,0.));
#8606=DIRECTION('center_axis',(0.,-1.,0.));
#8607=DIRECTION('ref_axis',(0.,0.,-1.));
#8608=DIRECTION('center_axis',(0.,-1.,0.));
#8609=DIRECTION('ref_axis',(0.,0.,-1.));
#8610=DIRECTION('center_axis',(0.,1.15648231731787E-16,-1.));
#8611=DIRECTION('ref_axis',(0.,1.,0.));
#8612=DIRECTION('axis',(0.,0.,1.));
#8613=DIRECTION('refdir',(1.,0.,0.));
#8614=DIRECTION('center_axis',(0.,-1.,0.));
#8615=DIRECTION('ref_axis',(0.,0.,-1.));
#8616=DIRECTION('center_axis',(0.,1.,0.));
#8617=DIRECTION('ref_axis',(0.,0.,1.));
#8618=DIRECTION('',(0.,-1.,0.));
#8619=DIRECTION('center_axis',(0.,-1.,0.));
#8620=DIRECTION('ref_axis',(0.,0.,-1.));
#8621=DIRECTION('center_axis',(0.,1.,0.));
#8622=DIRECTION('ref_axis',(0.,0.,1.));
#8623=DIRECTION('center_axis',(0.,-1.,0.));
#8624=DIRECTION('ref_axis',(0.,0.,-1.));
#8625=DIRECTION('',(0.,-1.,0.));
#8626=DIRECTION('center_axis',(0.,1.,0.));
#8627=DIRECTION('ref_axis',(0.,0.,-1.));
#8628=DIRECTION('center_axis',(0.,1.,0.));
#8629=DIRECTION('ref_axis',(0.,0.,1.));
#8630=DIRECTION('center_axis',(0.,-1.,0.));
#8631=DIRECTION('ref_axis',(0.,0.,1.));
#8632=DIRECTION('',(0.,-1.,0.));
#8633=DIRECTION('center_axis',(0.,-1.,0.));
#8634=DIRECTION('ref_axis',(0.,0.,-1.));
#8635=DIRECTION('center_axis',(0.,1.,0.));
#8636=DIRECTION('ref_axis',(0.,0.,1.));
#8637=DIRECTION('center_axis',(0.,-1.,0.));
#8638=DIRECTION('ref_axis',(0.,0.,1.));
#8639=DIRECTION('',(0.,-1.,0.));
#8640=DIRECTION('center_axis',(0.,1.,0.));
#8641=DIRECTION('ref_axis',(0.,0.,-1.));
#8642=DIRECTION('center_axis',(0.,-1.,0.));
#8643=DIRECTION('ref_axis',(0.,0.,-1.));
#8644=DIRECTION('center_axis',(0.,-1.,-1.24352412568707E-16));
#8645=DIRECTION('ref_axis',(0.,-1.24352412568707E-16,1.));
#8646=DIRECTION('',(0.,-1.,0.));
#8647=DIRECTION('center_axis',(0.,-1.,0.));
#8648=DIRECTION('ref_axis',(0.,0.,-1.));
#8649=DIRECTION('',(0.,-1.,0.));
#8650=DIRECTION('center_axis',(0.,1.,1.24352412568707E-16));
#8651=DIRECTION('ref_axis',(0.,1.24352412568707E-16,-1.));
#8652=DIRECTION('center_axis',(0.,0.,-1.));
#8653=DIRECTION('ref_axis',(1.,0.,0.));
#8654=DIRECTION('center_axis',(0.,0.,1.));
#8655=DIRECTION('ref_axis',(-1.,0.,0.));
#8656=DIRECTION('center_axis',(0.,0.,1.));
#8657=DIRECTION('ref_axis',(-1.,0.,0.));
#8658=DIRECTION('',(0.0174524064372835,-2.1373033680838E-18,0.999847695156391));
#8659=DIRECTION('center_axis',(0.,0.,1.));
#8660=DIRECTION('ref_axis',(-1.,0.,0.));
#8661=DIRECTION('center_axis',(0.,-1.,0.));
#8662=DIRECTION('ref_axis',(0.,0.,-1.));
#8663=DIRECTION('',(0.,-1.,0.));
#8664=DIRECTION('center_axis',(0.,1.,1.24352412568707E-16));
#8665=DIRECTION('ref_axis',(0.,1.24352412568707E-16,-1.));
#8666=DIRECTION('',(0.,1.,0.));
#8667=DIRECTION('center_axis',(0.,-1.,0.));
#8668=DIRECTION('ref_axis',(0.,0.,-1.));
#8669=DIRECTION('center_axis',(0.,-1.,-1.24352412568707E-16));
#8670=DIRECTION('ref_axis',(1.86381695289753E-15,-1.24352412568707E-16,
1.));
#8671=DIRECTION('',(0.,-1.,0.));
#8672=DIRECTION('',(0.,1.,0.));
#8673=DIRECTION('center_axis',(0.,1.15648231731787E-16,-1.));
#8674=DIRECTION('ref_axis',(0.,1.,0.));
#8675=DIRECTION('center_axis',(0.,1.15648231731787E-16,-1.));
#8676=DIRECTION('ref_axis',(0.,1.,1.15648231731787E-16));
#8677=DIRECTION('center_axis',(0.,-1.,0.));
#8678=DIRECTION('ref_axis',(0.,0.,-1.));
#8679=DIRECTION('center_axis',(0.,1.,1.24352412568707E-16));
#8680=DIRECTION('ref_axis',(0.,-1.24352412568707E-16,1.));
#8681=DIRECTION('',(0.,-1.,0.));
#8682=DIRECTION('',(0.,-1.,0.));
#8683=DIRECTION('center_axis',(0.,-1.,-1.24352412568707E-16));
#8684=DIRECTION('ref_axis',(0.,1.24352412568707E-16,-1.));
#8685=DIRECTION('',(0.,1.,0.));
#8686=DIRECTION('center_axis',(-0.707106781186547,0.,-0.707106781186548));
#8687=DIRECTION('ref_axis',(-0.707106781186548,0.,0.707106781186547));
#8688=DIRECTION('',(-0.707106781186548,0.,0.707106781186547));
#8689=DIRECTION('',(0.,1.,0.));
#8690=DIRECTION('',(-0.707106781186548,0.,0.707106781186547));
#8691=DIRECTION('',(0.,-1.,0.));
#8692=DIRECTION('center_axis',(0.,0.,-1.));
#8693=DIRECTION('ref_axis',(-1.,-1.22464679914735E-16,0.));
#8694=DIRECTION('center_axis',(0.,0.,-1.));
#8695=DIRECTION('ref_axis',(1.,1.77635684317072E-15,0.));
#8696=DIRECTION('center_axis',(0.,-1.,0.));
#8697=DIRECTION('ref_axis',(3.0760962761356E-5,0.,0.999999999526882));
#8698=DIRECTION('',(0.,1.,0.));
#8699=DIRECTION('center_axis',(0.,1.,0.));
#8700=DIRECTION('ref_axis',(2.66489596482314E-15,0.,-1.));
#8701=DIRECTION('',(0.,-1.,0.));
#8702=DIRECTION('center_axis',(0.,-1.,0.));
#8703=DIRECTION('ref_axis',(0.,0.,1.));
#8704=DIRECTION('center_axis',(0.,1.15648231731787E-16,-1.));
#8705=DIRECTION('ref_axis',(0.,1.,1.15648231731787E-16));
#8706=DIRECTION('',(-1.,0.,0.));
#8707=DIRECTION('',(0.,-1.,-1.15648231731787E-16));
#8708=DIRECTION('',(-1.,0.,0.));
#8709=DIRECTION('center_axis',(0.,1.,1.24352412568707E-16));
#8710=DIRECTION('ref_axis',(0.,-1.24352412568707E-16,1.));
#8711=DIRECTION('center_axis',(0.,-1.,-1.24352412568707E-16));
#8712=DIRECTION('ref_axis',(0.,-1.24352412568707E-16,1.));
#8713=DIRECTION('center_axis',(0.,1.,1.24352412568707E-16));
#8714=DIRECTION('ref_axis',(0.,-1.24352412568707E-16,1.));
#8715=DIRECTION('center_axis',(0.,1.,1.24352412568707E-16));
#8716=DIRECTION('ref_axis',(0.,-1.24352412568707E-16,1.));
#8717=DIRECTION('',(0.,1.24352412568707E-16,-1.));
#8718=DIRECTION('center_axis',(0.,-1.,-1.24352412568707E-16));
#8719=DIRECTION('ref_axis',(0.,1.24352412568707E-16,-1.));
#8720=DIRECTION('center_axis',(0.,-1.,-1.24352412568707E-16));
#8721=DIRECTION('ref_axis',(0.,1.24352412568707E-16,-1.));
#8722=DIRECTION('center_axis',(0.,1.,1.24352412568707E-16));
#8723=DIRECTION('ref_axis',(0.,1.24352412568707E-16,-1.));
#8724=DIRECTION('',(0.,-1.24352412568707E-16,1.));
#8725=DIRECTION('center_axis',(0.,-1.,-1.24352412568707E-16));
#8726=DIRECTION('ref_axis',(0.,1.24352412568707E-16,-1.));
#8727=DIRECTION('center_axis',(-1.,0.,0.));
#8728=DIRECTION('ref_axis',(0.,0.,1.));
#8729=DIRECTION('center_axis',(0.,0.,1.));
#8730=DIRECTION('ref_axis',(1.,0.,0.));
#8731=DIRECTION('',(-1.,0.,0.));
#8732=DIRECTION('',(0.,1.,0.));
#8733=DIRECTION('',(-1.,0.,0.));
#8734=DIRECTION('center_axis',(0.,-1.,0.));
#8735=DIRECTION('ref_axis',(0.,0.,-1.));
#8736=DIRECTION('',(0.707106781186548,0.,-0.707106781186547));
#8737=DIRECTION('center_axis',(0.,1.,0.));
#8738=DIRECTION('ref_axis',(0.,0.,-1.));
#8739=DIRECTION('',(0.707106781186548,0.,0.707106781186548));
#8740=DIRECTION('',(-1.,0.,0.));
#8741=DIRECTION('',(0.707106781186548,0.,0.707106781186548));
#8742=DIRECTION('center_axis',(0.,1.,0.));
#8743=DIRECTION('ref_axis',(-4.33680868994202E-15,0.,-1.));
#8744=DIRECTION('center_axis',(0.,0.,-1.));
#8745=DIRECTION('ref_axis',(-1.,0.,0.));
#8746=DIRECTION('',(0.,-1.,0.));
#8747=DIRECTION('',(-1.,0.,0.));
#8748=DIRECTION('center_axis',(0.,1.,0.));
#8749=DIRECTION('ref_axis',(0.,0.,1.));
#8750=DIRECTION('',(0.707106781186548,0.,0.707106781186548));
#8751=DIRECTION('center_axis',(0.,-1.,0.));
#8752=DIRECTION('ref_axis',(0.,0.,1.));
#8753=DIRECTION('center_axis',(0.,-1.,0.));
#8754=DIRECTION('ref_axis',(-2.16840434497101E-15,0.,1.));
#8755=DIRECTION('',(0.707106781186548,0.,0.707106781186548));
#8756=DIRECTION('center_axis',(-0.707106781186548,0.,0.707106781186547));
#8757=DIRECTION('ref_axis',(0.707106781186547,0.,0.707106781186548));
#8758=DIRECTION('',(0.,1.,0.));
#8759=DIRECTION('',(0.707106781186548,0.,0.707106781186548));
#8760=DIRECTION('',(0.,1.,0.));
#8761=DIRECTION('',(-0.707106781186548,0.,-0.707106781186548));
#8762=DIRECTION('',(0.,1.,0.));
#8763=DIRECTION('center_axis',(0.707106781186548,0.,-0.707106781186547));
#8764=DIRECTION('ref_axis',(-0.707106781186547,0.,-0.707106781186548));
#8765=DIRECTION('',(-0.707106781186548,0.,-0.707106781186548));
#8766=DIRECTION('',(0.,-1.,0.));
#8767=DIRECTION('',(0.707106781186548,0.,0.707106781186548));
#8768=DIRECTION('',(0.,-1.,0.));
#8769=DIRECTION('',(0.,-1.,0.));
#8770=DIRECTION('center_axis',(-0.707106781186547,0.,-0.707106781186548));
#8771=DIRECTION('ref_axis',(-0.707106781186548,0.,0.707106781186547));
#8772=DIRECTION('',(0.707106781186548,0.,-0.707106781186547));
#8773=DIRECTION('',(0.,1.,0.));
#8774=DIRECTION('',(0.,-1.,0.));
#8775=DIRECTION('center_axis',(0.707106781186548,0.,0.707106781186548));
#8776=DIRECTION('ref_axis',(0.707106781186548,0.,-0.707106781186548));
#8777=DIRECTION('',(-0.707106781186547,0.,0.707106781186547));
#8778=DIRECTION('',(0.,1.,0.));
#8779=DIRECTION('',(-0.707106781186547,0.,0.707106781186547));
#8780=DIRECTION('',(0.,-1.,0.));
#8781=DIRECTION('center_axis',(0.,-1.,0.));
#8782=DIRECTION('ref_axis',(0.,0.,-1.));
#8783=DIRECTION('center_axis',(0.,1.,0.));
#8784=DIRECTION('ref_axis',(-4.33680868994202E-15,0.,-1.));
#8785=DIRECTION('center_axis',(0.,-1.,0.));
#8786=DIRECTION('ref_axis',(0.,0.,-1.));
#8787=DIRECTION('center_axis',(0.,-1.,0.));
#8788=DIRECTION('ref_axis',(0.,0.,-1.));
#8789=DIRECTION('center_axis',(0.,1.,0.));
#8790=DIRECTION('ref_axis',(-4.33680868994202E-15,0.,-1.));
#8791=DIRECTION('center_axis',(0.,1.,0.));
#8792=DIRECTION('ref_axis',(0.,0.,1.));
#8793=DIRECTION('center_axis',(0.,-1.,0.));
#8794=DIRECTION('ref_axis',(0.,0.,1.));
#8795=DIRECTION('center_axis',(0.,-1.,0.));
#8796=DIRECTION('ref_axis',(-2.16840434497101E-15,0.,1.));
#8797=DIRECTION('center_axis',(0.,1.,0.));
#8798=DIRECTION('ref_axis',(0.,0.,1.));
#8799=DIRECTION('center_axis',(0.,1.,0.));
#8800=DIRECTION('ref_axis',(0.,0.,1.));
#8801=DIRECTION('center_axis',(0.,-1.,0.));
#8802=DIRECTION('ref_axis',(0.,0.,-1.));
#8803=DIRECTION('center_axis',(0.,-1.,0.));
#8804=DIRECTION('ref_axis',(0.,0.,-1.));
#8805=DIRECTION('center_axis',(0.,1.,0.));
#8806=DIRECTION('ref_axis',(0.,0.,1.));
#8807=DIRECTION('center_axis',(0.,-1.,0.));
#8808=DIRECTION('ref_axis',(0.,0.,-1.));
#8809=DIRECTION('center_axis',(0.,-1.,0.));
#8810=DIRECTION('ref_axis',(0.,0.,-1.));
#8811=DIRECTION('center_axis',(0.,1.,0.));
#8812=DIRECTION('ref_axis',(1.45473230946492E-15,0.,-1.));
#8813=DIRECTION('center_axis',(0.,1.,0.));
#8814=DIRECTION('ref_axis',(1.45473230946492E-15,0.,-1.));
#8815=DIRECTION('center_axis',(0.,1.,0.));
#8816=DIRECTION('ref_axis',(1.01064309961486E-15,0.,-1.));
#8817=DIRECTION('center_axis',(0.,0.,-1.));
#8818=DIRECTION('ref_axis',(-1.,0.,0.));
#8819=DIRECTION('',(1.,0.,0.));
#8820=DIRECTION('',(0.,1.,0.));
#8821=DIRECTION('',(-1.,0.,0.));
#8822=DIRECTION('',(0.,-1.,0.));
#8823=DIRECTION('center_axis',(0.,-1.,0.));
#8824=DIRECTION('ref_axis',(0.,0.,-1.));
#8825=DIRECTION('',(0.,0.,1.));
#8826=DIRECTION('center_axis',(0.,-1.,0.));
#8827=DIRECTION('ref_axis',(0.,0.,-1.));
#8828=DIRECTION('center_axis',(0.,-1.,0.));
#8829=DIRECTION('ref_axis',(0.,0.,-1.));
#8830=DIRECTION('',(0.,0.,1.));
#8831=DIRECTION('center_axis',(1.,0.,0.));
#8832=DIRECTION('ref_axis',(0.,0.,-1.));
#8833=DIRECTION('',(0.,0.,1.));
#8834=DIRECTION('',(0.,-1.,0.));
#8835=DIRECTION('center_axis',(0.,1.,0.));
#8836=DIRECTION('ref_axis',(0.,0.,1.));
#8837=DIRECTION('center_axis',(0.,1.,0.));
#8838=DIRECTION('ref_axis',(0.,0.,1.));
#8839=DIRECTION('',(0.,0.,1.));
#8840=DIRECTION('center_axis',(0.,1.,0.));
#8841=DIRECTION('ref_axis',(0.,0.,1.));
#8842=DIRECTION('center_axis',(-1.,0.,0.));
#8843=DIRECTION('ref_axis',(0.,0.,1.));
#8844=DIRECTION('',(0.,1.,0.));
#8845=DIRECTION('center_axis',(0.,-1.,0.));
#8846=DIRECTION('ref_axis',(0.,0.,-1.));
#8847=DIRECTION('center_axis',(0.,1.,0.));
#8848=DIRECTION('ref_axis',(0.,0.,1.));
#8849=DIRECTION('center_axis',(0.,-1.,0.));
#8850=DIRECTION('ref_axis',(0.,0.,-1.));
#8851=DIRECTION('center_axis',(0.,-1.,0.));
#8852=DIRECTION('ref_axis',(0.,0.,-1.));
#8853=DIRECTION('center_axis',(0.,-1.,0.));
#8854=DIRECTION('ref_axis',(0.,0.,-1.));
#8855=DIRECTION('center_axis',(0.,-1.,0.));
#8856=DIRECTION('ref_axis',(0.,0.,-1.));
#8857=DIRECTION('',(0.,1.,0.));
#8858=DIRECTION('center_axis',(0.,-1.,0.));
#8859=DIRECTION('ref_axis',(0.,0.,-1.));
#8860=DIRECTION('',(0.,1.,0.));
#8861=DIRECTION('center_axis',(0.,-1.,0.));
#8862=DIRECTION('ref_axis',(0.,0.,-1.));
#8863=DIRECTION('center_axis',(0.,-1.,0.));
#8864=DIRECTION('ref_axis',(0.,0.,-1.));
#8865=DIRECTION('axis',(0.,0.,1.));
#8866=DIRECTION('refdir',(1.,0.,0.));
#8867=DIRECTION('axis',(0.,0.,1.));
#8868=DIRECTION('refdir',(1.,0.,0.));
#8869=DIRECTION('center_axis',(0.,0.,1.));
#8870=DIRECTION('ref_axis',(1.,0.,0.));
#8871=DIRECTION('center_axis',(0.,0.,1.));
#8872=DIRECTION('ref_axis',(1.,0.,0.));
#8873=DIRECTION('',(0.,0.,1.));
#8874=DIRECTION('center_axis',(0.,0.,1.));
#8875=DIRECTION('ref_axis',(1.,0.,0.));
#8876=DIRECTION('center_axis',(1.,-1.0842021724855E-16,0.));
#8877=DIRECTION('ref_axis',(1.0842021724855E-16,1.,0.));
#8878=DIRECTION('center_axis',(1.,-7.2280144832367E-17,0.));
#8879=DIRECTION('ref_axis',(7.2280144832367E-17,1.,0.));
#8880=DIRECTION('',(1.,-1.0842021724855E-16,0.));
#8881=DIRECTION('center_axis',(1.,-1.0842021724855E-16,0.));
#8882=DIRECTION('ref_axis',(1.0842021724855E-16,1.,0.));
#8883=DIRECTION('center_axis',(0.,0.,-1.));
#8884=DIRECTION('ref_axis',(-1.,0.,0.));
#8885=DIRECTION('center_axis',(0.,0.,1.));
#8886=DIRECTION('ref_axis',(1.,0.,0.));
#8887=DIRECTION('',(0.,0.,1.));
#8888=DIRECTION('center_axis',(0.,0.,1.));
#8889=DIRECTION('ref_axis',(1.,0.,0.));
#8890=DIRECTION('center_axis',(0.,0.,1.));
#8891=DIRECTION('ref_axis',(1.,0.,0.));
#8892=DIRECTION('',(7.2280144832367E-17,1.,0.));
#8893=DIRECTION('',(-1.,0.,0.));
#8894=DIRECTION('',(-1.44560289664734E-16,-1.,0.));
#8895=DIRECTION('',(1.,0.,0.));
#8896=DIRECTION('center_axis',(0.,0.,1.));
#8897=DIRECTION('ref_axis',(1.,0.,0.));
#8898=DIRECTION('center_axis',(1.,-7.2280144832367E-17,0.));
#8899=DIRECTION('ref_axis',(7.2280144832367E-17,1.,0.));
#8900=DIRECTION('center_axis',(-1.,7.2280144832367E-17,0.));
#8901=DIRECTION('ref_axis',(7.2280144832367E-17,1.,0.));
#8902=DIRECTION('',(0.,0.,1.));
#8903=DIRECTION('',(0.,0.,1.));
#8904=DIRECTION('center_axis',(0.,-1.,0.));
#8905=DIRECTION('ref_axis',(0.,0.,-1.));
#8906=DIRECTION('',(0.,0.,1.));
#8907=DIRECTION('',(-1.,0.,0.));
#8908=DIRECTION('center_axis',(-1.,1.44560289664734E-16,0.));
#8909=DIRECTION('ref_axis',(-1.44560289664734E-16,-1.,0.));
#8910=DIRECTION('',(0.,0.,1.));
#8911=DIRECTION('center_axis',(1.,-1.44560289664734E-16,0.));
#8912=DIRECTION('ref_axis',(-1.44560289664734E-16,-1.,0.));
#8913=DIRECTION('center_axis',(0.,1.,0.));
#8914=DIRECTION('ref_axis',(0.,0.,1.));
#8915=DIRECTION('',(1.,0.,0.));
#8916=DIRECTION('center_axis',(-1.,0.,0.));
#8917=DIRECTION('ref_axis',(0.,1.22464679914735E-16,-1.));
#8918=DIRECTION('center_axis',(0.,0.,1.));
#8919=DIRECTION('ref_axis',(1.,0.,0.));
#8920=DIRECTION('axis',(0.,0.,1.));
#8921=DIRECTION('refdir',(1.,0.,0.));
#8922=DIRECTION('center_axis',(1.,1.23908819712629E-16,0.));
#8923=DIRECTION('ref_axis',(-1.23908819712629E-16,1.,0.));
#8924=DIRECTION('center_axis',(1.,1.23908819712629E-16,0.));
#8925=DIRECTION('ref_axis',(-1.23908819712629E-16,1.,0.));
#8926=DIRECTION('',(1.,1.23908819712629E-16,0.));
#8927=DIRECTION('center_axis',(1.,1.23908819712629E-16,0.));
#8928=DIRECTION('ref_axis',(-1.23908819712629E-16,1.,0.));
#8929=DIRECTION('center_axis',(1.,1.23908819712629E-16,0.));
#8930=DIRECTION('ref_axis',(-2.11060815823259E-32,6.12323399573677E-17,
1.));
#8931=DIRECTION('center_axis',(-1.,-1.23908819712629E-16,0.));
#8932=DIRECTION('ref_axis',(-1.23908819712629E-16,1.,0.));
#8933=DIRECTION('',(-1.,-1.23908819712629E-16,0.));
#8934=DIRECTION('center_axis',(1.,1.23908819712629E-16,0.));
#8935=DIRECTION('ref_axis',(-1.23908819712629E-16,1.,0.));
#8936=DIRECTION('',(1.,1.23908819712629E-16,0.));
#8937=DIRECTION('center_axis',(0.,0.,-1.));
#8938=DIRECTION('ref_axis',(-1.,0.,0.));
#8939=DIRECTION('center_axis',(0.,0.,1.));
#8940=DIRECTION('ref_axis',(1.,0.,0.));
#8941=DIRECTION('',(0.,0.,1.));
#8942=DIRECTION('center_axis',(0.,0.,1.));
#8943=DIRECTION('ref_axis',(1.,0.,0.));
#8944=DIRECTION('center_axis',(0.,0.,1.));
#8945=DIRECTION('ref_axis',(1.,0.,0.));
#8946=DIRECTION('',(-1.,0.,0.));
#8947=DIRECTION('',(-1.23908819712629E-16,1.,0.));
#8948=DIRECTION('',(1.,0.,0.));
#8949=DIRECTION('',(1.23908819712629E-16,-1.,0.));
#8950=DIRECTION('center_axis',(0.,0.,1.));
#8951=DIRECTION('ref_axis',(1.,0.,0.));
#8952=DIRECTION('center_axis',(-1.,-1.23908819712629E-16,0.));
#8953=DIRECTION('ref_axis',(1.23908819712629E-16,-1.,0.));
#8954=DIRECTION('',(0.,0.,-1.));
#8955=DIRECTION('',(0.,0.,-1.));
#8956=DIRECTION('center_axis',(0.,-1.,0.));
#8957=DIRECTION('ref_axis',(0.,0.,-1.));
#8958=DIRECTION('',(0.,0.,-1.));
#8959=DIRECTION('center_axis',(1.,1.23908819712629E-16,0.));
#8960=DIRECTION('ref_axis',(-1.23908819712629E-16,1.,0.));
#8961=DIRECTION('',(0.,0.,-1.));
#8962=DIRECTION('center_axis',(0.,1.,0.));
#8963=DIRECTION('ref_axis',(0.,0.,1.));
#8964=DIRECTION('',(4.93038065763132E-32,1.24728505009631E-31,1.));
#8965=DIRECTION('',(1.,2.46519032881566E-31,-4.93038065763132E-32));
#8966=DIRECTION('',(4.93038065763132E-32,1.24728505009631E-31,1.));
#8967=DIRECTION('',(1.,2.46519032881566E-31,-4.93038065763132E-32));
#8968=DIRECTION('axis',(0.,0.,1.));
#8969=DIRECTION('refdir',(1.,0.,0.));
#8970=DIRECTION('axis',(0.,0.,1.));
#8971=DIRECTION('refdir',(1.,0.,0.));
#8972=DIRECTION('center_axis',(0.,0.,1.));
#8973=DIRECTION('ref_axis',(1.,0.,0.));
#8974=DIRECTION('center_axis',(0.,0.,1.));
#8975=DIRECTION('ref_axis',(1.,0.,0.));
#8976=DIRECTION('',(0.,0.,1.));
#8977=DIRECTION('center_axis',(0.,0.,1.));
#8978=DIRECTION('ref_axis',(1.,0.,0.));
#8979=DIRECTION('center_axis',(1.,-1.0842021724855E-16,0.));
#8980=DIRECTION('ref_axis',(1.0842021724855E-16,1.,0.));
#8981=DIRECTION('center_axis',(1.,-7.2280144832367E-17,0.));
#8982=DIRECTION('ref_axis',(7.2280144832367E-17,1.,0.));
#8983=DIRECTION('',(1.,-1.0842021724855E-16,0.));
#8984=DIRECTION('center_axis',(1.,-1.0842021724855E-16,0.));
#8985=DIRECTION('ref_axis',(1.0842021724855E-16,1.,0.));
#8986=DIRECTION('center_axis',(0.,0.,-1.));
#8987=DIRECTION('ref_axis',(-1.,0.,0.));
#8988=DIRECTION('center_axis',(0.,0.,1.));
#8989=DIRECTION('ref_axis',(1.,0.,0.));
#8990=DIRECTION('',(0.,0.,1.));
#8991=DIRECTION('center_axis',(0.,0.,1.));
#8992=DIRECTION('ref_axis',(1.,0.,0.));
#8993=DIRECTION('center_axis',(0.,0.,1.));
#8994=DIRECTION('ref_axis',(1.,0.,0.));
#8995=DIRECTION('',(7.2280144832367E-17,1.,0.));
#8996=DIRECTION('',(-1.,0.,0.));
#8997=DIRECTION('',(-1.44560289664734E-16,-1.,0.));
#8998=DIRECTION('',(1.,0.,0.));
#8999=DIRECTION('center_axis',(0.,0.,1.));
#9000=DIRECTION('ref_axis',(1.,0.,0.));
#9001=DIRECTION('center_axis',(1.,-7.2280144832367E-17,0.));
#9002=DIRECTION('ref_axis',(7.2280144832367E-17,1.,0.));
#9003=DIRECTION('center_axis',(-1.,7.2280144832367E-17,0.));
#9004=DIRECTION('ref_axis',(7.2280144832367E-17,1.,0.));
#9005=DIRECTION('',(0.,0.,1.));
#9006=DIRECTION('',(0.,0.,1.));
#9007=DIRECTION('center_axis',(0.,-1.,0.));
#9008=DIRECTION('ref_axis',(0.,0.,-1.));
#9009=DIRECTION('',(0.,0.,1.));
#9010=DIRECTION('',(-1.,0.,0.));
#9011=DIRECTION('center_axis',(-1.,1.44560289664734E-16,0.));
#9012=DIRECTION('ref_axis',(-1.44560289664734E-16,-1.,0.));
#9013=DIRECTION('',(0.,0.,1.));
#9014=DIRECTION('center_axis',(1.,-1.44560289664734E-16,0.));
#9015=DIRECTION('ref_axis',(-1.44560289664734E-16,-1.,0.));
#9016=DIRECTION('center_axis',(0.,1.,0.));
#9017=DIRECTION('ref_axis',(0.,0.,1.));
#9018=DIRECTION('',(1.,0.,0.));
#9019=DIRECTION('center_axis',(-1.,0.,0.));
#9020=DIRECTION('ref_axis',(0.,1.22464679914735E-16,-1.));
#9021=DIRECTION('center_axis',(0.,0.,1.));
#9022=DIRECTION('ref_axis',(1.,0.,0.));
#9023=DIRECTION('axis',(0.,0.,1.));
#9024=DIRECTION('refdir',(1.,0.,0.));
#9025=DIRECTION('center_axis',(1.,1.23908819712629E-16,0.));
#9026=DIRECTION('ref_axis',(-1.23908819712629E-16,1.,0.));
#9027=DIRECTION('center_axis',(1.,1.23908819712629E-16,0.));
#9028=DIRECTION('ref_axis',(-1.23908819712629E-16,1.,0.));
#9029=DIRECTION('',(1.,1.23908819712629E-16,0.));
#9030=DIRECTION('center_axis',(1.,1.23908819712629E-16,0.));
#9031=DIRECTION('ref_axis',(-1.23908819712629E-16,1.,0.));
#9032=DIRECTION('center_axis',(1.,1.23908819712629E-16,0.));
#9033=DIRECTION('ref_axis',(-2.11060815823259E-32,6.12323399573677E-17,
1.));
#9034=DIRECTION('center_axis',(-1.,-1.23908819712629E-16,0.));
#9035=DIRECTION('ref_axis',(-1.23908819712629E-16,1.,0.));
#9036=DIRECTION('',(-1.,-1.23908819712629E-16,0.));
#9037=DIRECTION('center_axis',(1.,1.23908819712629E-16,0.));
#9038=DIRECTION('ref_axis',(-1.23908819712629E-16,1.,0.));
#9039=DIRECTION('',(1.,1.23908819712629E-16,0.));
#9040=DIRECTION('center_axis',(0.,0.,-1.));
#9041=DIRECTION('ref_axis',(-1.,0.,0.));
#9042=DIRECTION('center_axis',(0.,0.,1.));
#9043=DIRECTION('ref_axis',(1.,0.,0.));
#9044=DIRECTION('',(0.,0.,1.));
#9045=DIRECTION('center_axis',(0.,0.,1.));
#9046=DIRECTION('ref_axis',(1.,0.,0.));
#9047=DIRECTION('center_axis',(0.,0.,1.));
#9048=DIRECTION('ref_axis',(1.,0.,0.));
#9049=DIRECTION('',(-1.,0.,0.));
#9050=DIRECTION('',(-1.23908819712629E-16,1.,0.));
#9051=DIRECTION('',(1.,0.,0.));
#9052=DIRECTION('',(1.23908819712629E-16,-1.,0.));
#9053=DIRECTION('center_axis',(0.,0.,1.));
#9054=DIRECTION('ref_axis',(1.,0.,0.));
#9055=DIRECTION('center_axis',(-1.,-1.23908819712629E-16,0.));
#9056=DIRECTION('ref_axis',(1.23908819712629E-16,-1.,0.));
#9057=DIRECTION('',(0.,0.,-1.));
#9058=DIRECTION('',(0.,0.,-1.));
#9059=DIRECTION('center_axis',(0.,-1.,0.));
#9060=DIRECTION('ref_axis',(0.,0.,-1.));
#9061=DIRECTION('',(0.,0.,-1.));
#9062=DIRECTION('center_axis',(1.,1.23908819712629E-16,0.));
#9063=DIRECTION('ref_axis',(-1.23908819712629E-16,1.,0.));
#9064=DIRECTION('',(0.,0.,-1.));
#9065=DIRECTION('center_axis',(0.,1.,0.));
#9066=DIRECTION('ref_axis',(0.,0.,1.));
#9067=DIRECTION('',(9.86076131526264E-32,6.93889390390735E-18,1.));
#9068=DIRECTION('',(1.,-1.36845553156723E-48,-9.86076131526264E-32));
#9069=DIRECTION('',(9.86076131526264E-32,6.93889390390735E-18,1.));
#9070=DIRECTION('',(1.,-1.36845553156723E-48,-9.86076131526264E-32));
#9071=DIRECTION('axis',(0.,0.,1.));
#9072=DIRECTION('refdir',(1.,0.,0.));
#9073=DIRECTION('axis',(0.,0.,1.));
#9074=DIRECTION('refdir',(1.,0.,0.));
#9075=DIRECTION('center_axis',(0.,0.,1.));
#9076=DIRECTION('ref_axis',(1.,0.,0.));
#9077=DIRECTION('center_axis',(0.,0.,1.));
#9078=DIRECTION('ref_axis',(1.,0.,0.));
#9079=DIRECTION('',(0.,0.,1.));
#9080=DIRECTION('center_axis',(0.,0.,1.));
#9081=DIRECTION('ref_axis',(1.,0.,0.));
#9082=DIRECTION('center_axis',(1.,-1.0842021724855E-16,0.));
#9083=DIRECTION('ref_axis',(1.0842021724855E-16,1.,0.));
#9084=DIRECTION('center_axis',(1.,-7.2280144832367E-17,0.));
#9085=DIRECTION('ref_axis',(7.2280144832367E-17,1.,0.));
#9086=DIRECTION('',(1.,-1.0842021724855E-16,0.));
#9087=DIRECTION('center_axis',(1.,-1.0842021724855E-16,0.));
#9088=DIRECTION('ref_axis',(1.0842021724855E-16,1.,0.));
#9089=DIRECTION('center_axis',(0.,0.,-1.));
#9090=DIRECTION('ref_axis',(-1.,0.,0.));
#9091=DIRECTION('center_axis',(0.,0.,1.));
#9092=DIRECTION('ref_axis',(1.,0.,0.));
#9093=DIRECTION('',(0.,0.,1.));
#9094=DIRECTION('center_axis',(0.,0.,1.));
#9095=DIRECTION('ref_axis',(1.,0.,0.));
#9096=DIRECTION('center_axis',(0.,0.,1.));
#9097=DIRECTION('ref_axis',(1.,0.,0.));
#9098=DIRECTION('',(7.2280144832367E-17,1.,0.));
#9099=DIRECTION('',(-1.,0.,0.));
#9100=DIRECTION('',(-1.44560289664734E-16,-1.,0.));
#9101=DIRECTION('',(1.,0.,0.));
#9102=DIRECTION('center_axis',(0.,0.,1.));
#9103=DIRECTION('ref_axis',(1.,0.,0.));
#9104=DIRECTION('center_axis',(1.,-7.2280144832367E-17,0.));
#9105=DIRECTION('ref_axis',(7.2280144832367E-17,1.,0.));
#9106=DIRECTION('center_axis',(-1.,7.2280144832367E-17,0.));
#9107=DIRECTION('ref_axis',(7.22801448323669E-17,1.,0.));
#9108=DIRECTION('',(0.,0.,1.));
#9109=DIRECTION('',(0.,0.,1.));
#9110=DIRECTION('center_axis',(0.,-1.,0.));
#9111=DIRECTION('ref_axis',(0.,0.,-1.));
#9112=DIRECTION('',(0.,0.,1.));
#9113=DIRECTION('',(-1.,0.,0.));
#9114=DIRECTION('center_axis',(-1.,1.44560289664734E-16,0.));
#9115=DIRECTION('ref_axis',(-1.44560289664734E-16,-1.,0.));
#9116=DIRECTION('',(0.,0.,1.));
#9117=DIRECTION('center_axis',(1.,-1.44560289664734E-16,0.));
#9118=DIRECTION('ref_axis',(-1.44560289664734E-16,-1.,0.));
#9119=DIRECTION('center_axis',(0.,1.,0.));
#9120=DIRECTION('ref_axis',(0.,0.,1.));
#9121=DIRECTION('',(1.,0.,0.));
#9122=DIRECTION('center_axis',(-1.,0.,0.));
#9123=DIRECTION('ref_axis',(0.,1.22464679914735E-16,-1.));
#9124=DIRECTION('center_axis',(0.,0.,1.));
#9125=DIRECTION('ref_axis',(1.,0.,0.));
#9126=DIRECTION('axis',(0.,0.,1.));
#9127=DIRECTION('refdir',(1.,0.,0.));
#9128=DIRECTION('center_axis',(1.,1.23908819712629E-16,0.));
#9129=DIRECTION('ref_axis',(-1.23908819712629E-16,1.,0.));
#9130=DIRECTION('center_axis',(1.,1.23908819712629E-16,0.));
#9131=DIRECTION('ref_axis',(-1.23908819712629E-16,1.,0.));
#9132=DIRECTION('',(1.,1.23908819712629E-16,0.));
#9133=DIRECTION('center_axis',(1.,1.23908819712629E-16,0.));
#9134=DIRECTION('ref_axis',(-1.23908819712629E-16,1.,0.));
#9135=DIRECTION('center_axis',(1.,1.23908819712629E-16,0.));
#9136=DIRECTION('ref_axis',(-1.54074395550979E-32,6.12323399573677E-17,
1.));
#9137=DIRECTION('center_axis',(-1.,-1.23908819712629E-16,0.));
#9138=DIRECTION('ref_axis',(-1.23908819712629E-16,1.,0.));
#9139=DIRECTION('',(-1.,-1.23908819712629E-16,0.));
#9140=DIRECTION('center_axis',(1.,1.23908819712629E-16,0.));
#9141=DIRECTION('ref_axis',(-1.23908819712629E-16,1.,0.));
#9142=DIRECTION('',(1.,1.23908819712629E-16,0.));
#9143=DIRECTION('center_axis',(0.,0.,-1.));
#9144=DIRECTION('ref_axis',(-1.,-4.93038065763131E-32,0.));
#9145=DIRECTION('center_axis',(0.,0.,1.));
#9146=DIRECTION('ref_axis',(1.,4.93038065763131E-32,0.));
#9147=DIRECTION('',(0.,0.,1.));
#9148=DIRECTION('center_axis',(0.,0.,1.));
#9149=DIRECTION('ref_axis',(1.,4.93038065763131E-32,0.));
#9150=DIRECTION('center_axis',(0.,0.,1.));
#9151=DIRECTION('ref_axis',(1.,4.93038065763131E-32,0.));
#9152=DIRECTION('',(-1.,-4.93038065763131E-32,0.));
#9153=DIRECTION('',(-1.23908819712629E-16,1.,0.));
#9154=DIRECTION('',(1.,4.93038065763131E-32,0.));
#9155=DIRECTION('',(1.23908819712629E-16,-1.,0.));
#9156=DIRECTION('center_axis',(0.,0.,1.));
#9157=DIRECTION('ref_axis',(1.,4.93038065763131E-32,0.));
#9158=DIRECTION('center_axis',(-1.,-1.23908819712629E-16,0.));
#9159=DIRECTION('ref_axis',(1.23908819712629E-16,-1.,0.));
#9160=DIRECTION('',(0.,0.,-1.));
#9161=DIRECTION('',(0.,0.,-1.));
#9162=DIRECTION('center_axis',(4.93038065763131E-32,-1.,0.));
#9163=DIRECTION('ref_axis',(0.,0.,-1.));
#9164=DIRECTION('',(0.,0.,-1.));
#9165=DIRECTION('center_axis',(1.,1.23908819712629E-16,0.));
#9166=DIRECTION('ref_axis',(-1.23908819712629E-16,1.,0.));
#9167=DIRECTION('',(0.,0.,-1.));
#9168=DIRECTION('center_axis',(-4.93038065763131E-32,1.,0.));
#9169=DIRECTION('ref_axis',(0.,0.,1.));
#9170=DIRECTION('axis',(0.,0.,1.));
#9171=DIRECTION('refdir',(1.,0.,0.));
#9172=DIRECTION('center_axis',(-1.,0.,0.));
#9173=DIRECTION('ref_axis',(0.,0.,1.));
#9174=DIRECTION('center_axis',(1.,0.,0.));
#9175=DIRECTION('ref_axis',(0.,0.,1.));
#9176=DIRECTION('',(1.,0.,0.));
#9177=DIRECTION('center_axis',(1.,0.,0.));
#9178=DIRECTION('ref_axis',(0.,0.,-1.));
#9179=DIRECTION('center_axis',(-1.,0.,0.));
#9180=DIRECTION('ref_axis',(0.,0.,1.));
#9181=DIRECTION('center_axis',(1.,0.,0.));
#9182=DIRECTION('ref_axis',(0.,0.,-1.));
#9183=DIRECTION('',(1.,0.,0.));
#9184=DIRECTION('center_axis',(-1.,0.,0.));
#9185=DIRECTION('ref_axis',(0.,0.,-1.));
#9186=DIRECTION('center_axis',(-1.,0.,0.));
#9187=DIRECTION('ref_axis',(0.,0.,1.));
#9188=DIRECTION('center_axis',(1.,0.,0.));
#9189=DIRECTION('ref_axis',(0.,0.,1.));
#9190=DIRECTION('',(1.,0.,0.));
#9191=DIRECTION('center_axis',(-1.,0.,0.));
#9192=DIRECTION('ref_axis',(0.,0.,-1.));
#9193=DIRECTION('center_axis',(0.,0.707106781186547,0.707106781186548));
#9194=DIRECTION('ref_axis',(0.,-0.707106781186548,0.707106781186547));
#9195=DIRECTION('',(0.,0.707106781186548,-0.707106781186547));
#9196=DIRECTION('',(1.,0.,0.));
#9197=DIRECTION('',(0.,0.707106781186548,-0.707106781186547));
#9198=DIRECTION('',(-1.,0.,0.));
#9199=DIRECTION('center_axis',(-1.,0.,0.));
#9200=DIRECTION('ref_axis',(0.,0.,1.));
#9201=DIRECTION('',(0.,0.,-1.));
#9202=DIRECTION('',(0.,-1.,0.));
#9203=DIRECTION('',(0.,-0.707106781186547,-0.707106781186548));
#9204=DIRECTION('',(0.,-0.707106781186547,-0.707106781186548));
#9205=DIRECTION('',(0.,-1.,0.));
#9206=DIRECTION('center_axis',(0.,0.,1.));
#9207=DIRECTION('ref_axis',(1.,0.,0.));
#9208=DIRECTION('',(-1.,0.,0.));
#9209=DIRECTION('',(0.,-1.,0.));
#9210=DIRECTION('',(-1.,0.,0.));
#9211=DIRECTION('center_axis',(1.,0.,0.));
#9212=DIRECTION('ref_axis',(0.,0.,-1.));
#9213=DIRECTION('',(0.,0.,1.));
#9214=DIRECTION('',(0.,-1.,0.));
#9215=DIRECTION('',(0.,-0.707106781186547,-0.707106781186548));
#9216=DIRECTION('',(0.,-0.707106781186548,0.707106781186547));
#9217=DIRECTION('',(0.,-0.707106781186547,-0.707106781186548));
#9218=DIRECTION('center_axis',(0.,0.,-1.));
#9219=DIRECTION('ref_axis',(-1.,0.,0.));
#9220=DIRECTION('',(1.,0.,0.));
#9221=DIRECTION('',(1.,0.,0.));
#9222=DIRECTION('center_axis',(0.,-1.,0.));
#9223=DIRECTION('ref_axis',(0.,0.,-1.));
#9224=DIRECTION('center_axis',(0.,0.707106781186548,-0.707106781186547));
#9225=DIRECTION('ref_axis',(0.,0.707106781186547,0.707106781186548));
#9226=DIRECTION('',(0.,0.707106781186547,0.707106781186548));
#9227=DIRECTION('',(1.,0.,0.));
#9228=DIRECTION('',(0.,-0.707106781186547,-0.707106781186548));
#9229=DIRECTION('',(1.,0.,0.));
#9230=DIRECTION('center_axis',(0.,-0.707106781186548,0.707106781186547));
#9231=DIRECTION('ref_axis',(0.,-0.707106781186547,-0.707106781186548));
#9232=DIRECTION('',(-1.,0.,0.));
#9233=DIRECTION('',(0.,-0.707106781186547,-0.707106781186547));
#9234=DIRECTION('',(-1.,0.,0.));
#9235=DIRECTION('',(0.,0.707106781186547,0.707106781186547));
#9236=DIRECTION('center_axis',(0.,0.707106781186547,0.707106781186548));
#9237=DIRECTION('ref_axis',(0.,-0.707106781186548,0.707106781186547));
#9238=DIRECTION('',(0.,-0.707106781186548,0.707106781186547));
#9239=DIRECTION('center_axis',(1.,0.,0.));
#9240=DIRECTION('ref_axis',(0.,0.,-1.));
#9241=DIRECTION('',(0.,0.707106781186548,-0.707106781186548));
#9242=DIRECTION('center_axis',(-1.,0.,0.));
#9243=DIRECTION('ref_axis',(0.,0.,1.));
#9244=DIRECTION('',(0.,0.707106781186548,-0.707106781186548));
#9245=DIRECTION('center_axis',(0.,-0.707106781186548,-0.707106781186548));
#9246=DIRECTION('ref_axis',(0.,0.707106781186548,-0.707106781186548));
#9247=DIRECTION('center_axis',(1.,0.,0.));
#9248=DIRECTION('ref_axis',(0.,0.,-1.));
#9249=DIRECTION('center_axis',(1.,0.,0.));
#9250=DIRECTION('ref_axis',(0.,0.,-1.));
#9251=DIRECTION('',(-1.6311770810255E-110,1.38503351396469E-31,1.));
#9252=DIRECTION('',(1.,6.82874244742263E-63,-9.45803714791358E-94));
#9253=DIRECTION('',(1.6552263248197E-17,3.37403716077489E-16,1.));
#9254=DIRECTION('',(-1.,1.18349050433848E-16,1.65522632481969E-17));
#9255=DIRECTION('',(-2.33209855411066E-16,-0.00403805980944622,0.999991847003252));
#9256=DIRECTION('',(1.,-6.52596544329667E-16,2.30576511423173E-16));
#9257=DIRECTION('axis',(0.,0.,1.));
#9258=DIRECTION('refdir',(1.,0.,0.));
#9259=DIRECTION('center_axis',(-1.,0.,0.));
#9260=DIRECTION('ref_axis',(0.,0.,1.));
#9261=DIRECTION('center_axis',(1.,0.,3.64131712001849E-16));
#9262=DIRECTION('ref_axis',(-3.64131712001849E-16,0.,1.));
#9263=DIRECTION('',(-1.,0.,0.));
#9264=DIRECTION('center_axis',(-1.,0.,0.));
#9265=DIRECTION('ref_axis',(0.,0.,1.));
#9266=DIRECTION('',(-1.,0.,0.));
#9267=DIRECTION('center_axis',(-1.,0.,-2.91305369601479E-16));
#9268=DIRECTION('ref_axis',(2.91305369601479E-16,0.,-1.));
#9269=DIRECTION('center_axis',(0.,-1.,0.));
#9270=DIRECTION('ref_axis',(0.,0.,-1.));
#9271=DIRECTION('center_axis',(-1.,0.,-2.23423785287372E-16));
#9272=DIRECTION('ref_axis',(-2.23423785287372E-16,0.,1.));
#9273=DIRECTION('center_axis',(-1.,0.,0.));
#9274=DIRECTION('ref_axis',(0.,0.,1.));
#9275=DIRECTION('center_axis',(-1.,0.,-2.91305369601479E-16));
#9276=DIRECTION('ref_axis',(2.91305369601479E-16,-1.73472347597681E-15,
-1.));
#9277=DIRECTION('',(-1.,0.,0.));
#9278=DIRECTION('center_axis',(1.,0.,3.64131712001849E-16));
#9279=DIRECTION('ref_axis',(-3.64131712001849E-16,-3.46944695195361E-15,
1.));
#9280=DIRECTION('',(1.,0.,0.));
#9281=DIRECTION('center_axis',(0.,-1.,0.));
#9282=DIRECTION('ref_axis',(0.,0.,-1.));
#9283=DIRECTION('',(-2.91305369601479E-16,0.,1.));
#9284=DIRECTION('',(-1.,0.,0.));
#9285=DIRECTION('',(3.64131712001849E-16,0.,-1.));
#9286=DIRECTION('',(1.,0.,0.));
#9287=DIRECTION('center_axis',(0.,0.,1.));
#9288=DIRECTION('ref_axis',(1.,0.,0.));
#9289=DIRECTION('',(0.,-1.,0.));
#9290=DIRECTION('',(0.,-1.,0.));
#9291=DIRECTION('center_axis',(-1.,0.,-3.64131712001849E-16));
#9292=DIRECTION('ref_axis',(-3.64131712001849E-16,0.,1.));
#9293=DIRECTION('',(0.,-1.,0.));
#9294=DIRECTION('center_axis',(0.,0.,-1.));
#9295=DIRECTION('ref_axis',(-1.,0.,0.));
#9296=DIRECTION('',(0.,-1.,0.));
#9297=DIRECTION('center_axis',(1.,0.,2.91305369601479E-16));
#9298=DIRECTION('ref_axis',(2.91305369601479E-16,0.,-1.));
#9299=DIRECTION('',(1.90471813372885E-33,-6.93334779979405E-32,1.));
#9300=DIRECTION('',(1.,-9.86076131526265E-32,-1.90471813372885E-33));
#9301=DIRECTION('',(0.706402654933587,2.23073171699748E-23,0.707810206978382));
#9302=DIRECTION('',(0.707810206978382,-5.92475125728477E-23,-0.706402654933587));
#9303=DIRECTION('',(0.981435379589937,-1.45777405041049E-21,-0.191793106469332));
#9304=DIRECTION('',(-0.191793106469332,-6.13017457408584E-21,-0.981435379589937));
#9305=DIRECTION('',(-0.0105320860142701,-2.95270034312141E-16,0.999944536043969));
#9306=DIRECTION('',(1.32313589782422E-16,-1.,-2.93892796660848E-16));
#9307=DIRECTION('',(0.720088610590378,-1.44499066804255E-16,0.693882117436398));
#9308=DIRECTION('',(-2.49902965017795E-18,-1.,-2.05653871788552E-16));
#9309=DIRECTION('',(-0.650979332105511,-1.08346481658803E-16,0.759095454584905));
#9310=DIRECTION('',(2.77555756156288E-17,1.,1.66533453693773E-16));
#9311=DIRECTION('',(0.191793106469332,4.69032157744452E-16,0.981435379589937));
#9312=DIRECTION('',(-1.11022302462516E-16,-1.,4.9960036108132E-16));
#9313=DIRECTION('axis',(0.,0.,1.));
#9314=DIRECTION('refdir',(1.,0.,0.));
#9315=DIRECTION('axis',(0.,0.,1.));
#9316=DIRECTION('refdir',(1.,0.,0.));
#9317=DIRECTION('center_axis',(0.,-0.224951054343868,0.974370064785235));
#9318=DIRECTION('ref_axis',(0.,-0.974370064785235,-0.224951054343868));
#9319=DIRECTION('center_axis',(0.,-0.224951054343868,0.974370064785235));
#9320=DIRECTION('ref_axis',(0.,-0.974370064785235,-0.224951054343868));
#9321=DIRECTION('',(0.,0.224951054343868,-0.974370064785235));
#9322=DIRECTION('center_axis',(0.,-0.224951054343868,0.974370064785235));
#9323=DIRECTION('ref_axis',(0.,0.974370064785235,0.224951054343868));
#9324=DIRECTION('center_axis',(0.,-0.224951054343865,0.974370064785235));
#9325=DIRECTION('ref_axis',(0.,-0.974370064785235,-0.224951054343865));
#9326=DIRECTION('center_axis',(0.,-0.224951054343865,0.974370064785235));
#9327=DIRECTION('ref_axis',(0.,-0.974370064785235,-0.224951054343865));
#9328=DIRECTION('',(0.,-0.224951054343865,0.974370064785235));
#9329=DIRECTION('center_axis',(0.,-0.224951054343865,0.974370064785235));
#9330=DIRECTION('ref_axis',(0.,-0.974370064785235,-0.224951054343865));
#9331=DIRECTION('center_axis',(0.,0.,-1.));
#9332=DIRECTION('ref_axis',(-1.,0.,0.));
#9333=DIRECTION('center_axis',(0.,1.1019100660974E-16,-1.));
#9334=DIRECTION('ref_axis',(0.,-1.,-1.1019100660974E-16));
#9335=DIRECTION('',(0.,0.,-1.));
#9336=DIRECTION('center_axis',(0.,0.,-1.));
#9337=DIRECTION('ref_axis',(1.,0.,0.));
#9338=DIRECTION('center_axis',(0.,0.,-1.));
#9339=DIRECTION('ref_axis',(-1.,0.,0.));
#9340=DIRECTION('center_axis',(0.,0.,1.));
#9341=DIRECTION('ref_axis',(-1.,0.,0.));
#9342=DIRECTION('',(0.,0.,-1.));
#9343=DIRECTION('center_axis',(0.,-9.18258388414501E-17,1.));
#9344=DIRECTION('ref_axis',(0.,1.,9.18258388414501E-17));
#9345=DIRECTION('center_axis',(-6.12323399573677E-17,0.,-1.));
#9346=DIRECTION('ref_axis',(-1.,0.,0.));
#9347=DIRECTION('center_axis',(-1.26882631385732E-16,-1.,0.));
#9348=DIRECTION('ref_axis',(1.,-1.26882631385732E-16,0.));
#9349=DIRECTION('center_axis',(0.,-1.1019100660974E-16,1.));
#9350=DIRECTION('ref_axis',(0.,-1.,-1.1019100660974E-16));
#9351=DIRECTION('center_axis',(1.,0.,0.));
#9352=DIRECTION('ref_axis',(0.,0.,-1.));
#9353=DIRECTION('center_axis',(0.,9.18258388414501E-17,-1.));
#9354=DIRECTION('ref_axis',(0.,1.,9.18258388414501E-17));
#9355=DIRECTION('center_axis',(-1.26882631385732E-16,-1.,0.));
#9356=DIRECTION('ref_axis',(1.,-1.26882631385732E-16,0.));
#9357=DIRECTION('center_axis',(0.,9.18258388414501E-17,-1.));
#9358=DIRECTION('ref_axis',(0.,1.,9.18258388414501E-17));
#9359=DIRECTION('center_axis',(0.,-1.,0.));
#9360=DIRECTION('ref_axis',(0.,0.,-1.));
#9361=DIRECTION('center_axis',(0.,-1.1019100660974E-16,1.));
#9362=DIRECTION('ref_axis',(0.,-1.,-1.1019100660974E-16));
#9363=DIRECTION('center_axis',(1.,0.,0.));
#9364=DIRECTION('ref_axis',(0.,0.,-1.));
#9365=DIRECTION('center_axis',(0.,-0.224951054343868,0.974370064785235));
#9366=DIRECTION('ref_axis',(0.,-0.974370064785235,-0.224951054343868));
#9367=DIRECTION('center_axis',(-1.,0.,0.));
#9368=DIRECTION('ref_axis',(0.,0.,1.));
#9369=DIRECTION('center_axis',(0.,0.224951054343868,-0.974370064785235));
#9370=DIRECTION('ref_axis',(0.,0.974370064785235,0.224951054343868));
#9371=DIRECTION('center_axis',(0.,0.974370064785235,0.224951054343868));
#9372=DIRECTION('ref_axis',(0.,-0.224951054343868,0.974370064785235));
#9373=DIRECTION('center_axis',(0.,-0.224951054343865,0.974370064785235));
#9374=DIRECTION('ref_axis',(0.,-0.974370064785235,-0.224951054343865));
#9375=DIRECTION('center_axis',(0.,0.974370064785235,0.224951054343868));
#9376=DIRECTION('ref_axis',(0.,-0.224951054343868,0.974370064785235));
#9377=DIRECTION('center_axis',(0.,-0.224951054343865,0.974370064785235));
#9378=DIRECTION('ref_axis',(0.,-0.974370064785235,-0.224951054343865));
#9379=DIRECTION('center_axis',(0.,0.974370064785235,0.224951054343868));
#9380=DIRECTION('ref_axis',(0.,-0.224951054343868,0.974370064785235));
#9381=DIRECTION('',(1.,0.,0.));
#9382=DIRECTION('',(0.,-0.224951054343868,0.974370064785235));
#9383=DIRECTION('',(1.,0.,0.));
#9384=DIRECTION('',(0.,0.224951054343868,-0.974370064785235));
#9385=DIRECTION('center_axis',(0.,0.974370064785235,0.224951054343868));
#9386=DIRECTION('ref_axis',(0.,-0.224951054343868,0.974370064785235));
#9387=DIRECTION('',(1.,0.,0.));
#9388=DIRECTION('',(0.,-0.224951054343868,0.974370064785235));
#9389=DIRECTION('',(1.,0.,0.));
#9390=DIRECTION('center_axis',(0.,-0.224951054343865,0.974370064785235));
#9391=DIRECTION('ref_axis',(0.,-0.974370064785235,-0.224951054343865));
#9392=DIRECTION('',(1.,0.,0.));
#9393=DIRECTION('',(0.,-0.974370064785235,-0.224951054343865));
#9394=DIRECTION('center_axis',(0.,0.974370064785235,0.224951054343868));
#9395=DIRECTION('ref_axis',(0.,-0.224951054343868,0.974370064785235));
#9396=DIRECTION('',(1.,0.,0.));
#9397=DIRECTION('',(0.,-0.224951054343868,0.974370064785235));
#9398=DIRECTION('center_axis',(0.,-0.224951054343865,0.974370064785235));
#9399=DIRECTION('ref_axis',(0.,-0.974370064785235,-0.224951054343865));
#9400=DIRECTION('',(0.,-0.974370064785235,-0.224951054343865));
#9401=DIRECTION('center_axis',(1.,0.,0.));
#9402=DIRECTION('ref_axis',(0.,0.,-1.));
#9403=DIRECTION('center_axis',(0.,-1.1019100660974E-16,1.));
#9404=DIRECTION('ref_axis',(0.,-1.,-1.1019100660974E-16));
#9405=DIRECTION('',(-1.,0.,0.));
#9406=DIRECTION('',(0.,1.,1.1019100660974E-16));
#9407=DIRECTION('center_axis',(0.,-1.,0.));
#9408=DIRECTION('ref_axis',(0.,0.,-1.));
#9409=DIRECTION('',(-1.,0.,0.));
#9410=DIRECTION('',(0.,0.,1.));
#9411=DIRECTION('center_axis',(0.,9.18258388414501E-17,-1.));
#9412=DIRECTION('ref_axis',(0.,1.,9.18258388414501E-17));
#9413=DIRECTION('',(0.,-1.,-9.18258388414501E-17));
#9414=DIRECTION('center_axis',(1.,0.,0.));
#9415=DIRECTION('ref_axis',(0.,0.,-1.));
#9416=DIRECTION('center_axis',(-1.,0.,0.));
#9417=DIRECTION('ref_axis',(0.,0.,1.));
#9418=DIRECTION('',(0.,-0.224951054343867,0.974370064785235));
#9419=DIRECTION('',(0.,0.974370064785235,0.224951054343868));
#9420=DIRECTION('',(0.,-0.974370064785235,-0.224951054343868));
#9421=DIRECTION('',(0.,-0.974370064785235,-0.224951054343868));
#9422=DIRECTION('',(0.,0.224951054343868,-0.974370064785235));
#9423=DIRECTION('',(0.,-0.974370064785235,-0.224951054343868));
#9424=DIRECTION('center_axis',(0.,-0.224951054343868,0.974370064785235));
#9425=DIRECTION('ref_axis',(0.,-0.974370064785235,-0.224951054343868));
#9426=DIRECTION('',(0.,-0.974370064785235,-0.224951054343868));
#9427=DIRECTION('',(-1.,0.,0.));
#9428=DIRECTION('center_axis',(1.,0.,0.));
#9429=DIRECTION('ref_axis',(0.,0.,-1.));
#9430=DIRECTION('',(0.,0.974370064785235,0.224951054343868));
#9431=DIRECTION('',(0.,-0.224951054343867,0.974370064785235));
#9432=DIRECTION('',(0.,-0.974370064785235,-0.224951054343868));
#9433=DIRECTION('',(0.,-0.224951054343868,0.974370064785235));
#9434=DIRECTION('',(0.,-0.974370064785235,-0.224951054343868));
#9435=DIRECTION('center_axis',(0.,0.224951054343868,-0.974370064785235));
#9436=DIRECTION('ref_axis',(0.,0.974370064785235,0.224951054343868));
#9437=DIRECTION('center_axis',(0.,0.974370064785235,0.224951054343868));
#9438=DIRECTION('ref_axis',(0.,-0.224951054343868,0.974370064785235));
#9439=DIRECTION('',(-1.,0.,0.));
#9440=DIRECTION('center_axis',(0.,-0.974370064785235,-0.224951054343867));
#9441=DIRECTION('ref_axis',(0.,0.224951054343867,-0.974370064785235));
#9442=DIRECTION('',(-1.,0.,0.));
#9443=DIRECTION('',(-1.,0.,0.));
#9444=DIRECTION('center_axis',(0.,-0.224951054343868,0.974370064785235));
#9445=DIRECTION('ref_axis',(0.,-0.974370064785235,-0.224951054343868));
#9446=DIRECTION('center_axis',(0.,0.224951054343868,-0.974370064785235));
#9447=DIRECTION('ref_axis',(0.,0.974370064785235,0.224951054343868));
#9448=DIRECTION('axis',(0.,0.,1.));
#9449=DIRECTION('refdir',(1.,0.,0.));
#9450=DIRECTION('center_axis',(0.,1.,0.));
#9451=DIRECTION('ref_axis',(0.,0.,1.));
#9452=DIRECTION('center_axis',(0.,1.,0.));
#9453=DIRECTION('ref_axis',(0.,0.,1.));
#9454=DIRECTION('',(0.,1.,0.));
#9455=DIRECTION('center_axis',(0.,1.,0.));
#9456=DIRECTION('ref_axis',(0.,0.,1.));
#9457=DIRECTION('center_axis',(0.,-1.,0.));
#9458=DIRECTION('ref_axis',(0.,0.,-1.));
#9459=DIRECTION('center_axis',(0.,-1.,-1.24352412568707E-16));
#9460=DIRECTION('ref_axis',(0.,-1.24352412568707E-16,1.));
#9461=DIRECTION('',(0.,-1.,0.));
#9462=DIRECTION('center_axis',(0.,-1.,0.));
#9463=DIRECTION('ref_axis',(0.,0.,-1.));
#9464=DIRECTION('',(0.,-1.,0.));
#9465=DIRECTION('center_axis',(0.,1.,1.24352412568707E-16));
#9466=DIRECTION('ref_axis',(0.,1.24352412568707E-16,-1.));
#9467=DIRECTION('center_axis',(0.,0.,1.));
#9468=DIRECTION('ref_axis',(1.,0.,0.));
#9469=DIRECTION('',(0.,1.,0.));
#9470=DIRECTION('',(-1.,0.,0.));
#9471=DIRECTION('',(0.,-1.,0.));
#9472=DIRECTION('center_axis',(0.,0.,1.));
#9473=DIRECTION('ref_axis',(1.,0.,0.));
#9474=DIRECTION('center_axis',(0.,-1.,0.));
#9475=DIRECTION('ref_axis',(0.,0.,-1.));
#9476=DIRECTION('',(0.,1.,0.));
#9477=DIRECTION('center_axis',(0.,-1.,0.));
#9478=DIRECTION('ref_axis',(-4.44101590494474E-15,0.,1.));
#9479=DIRECTION('',(0.,-1.,0.));
#9480=DIRECTION('',(0.,1.,0.));
#9481=DIRECTION('center_axis',(0.,-1.,0.));
#9482=DIRECTION('ref_axis',(-4.44101590494474E-15,0.,1.));
#9483=DIRECTION('center_axis',(0.,-1.,0.));
#9484=DIRECTION('ref_axis',(0.,0.,-1.));
#9485=DIRECTION('center_axis',(0.,-1.,0.));
#9486=DIRECTION('ref_axis',(0.,0.,1.));
#9487=DIRECTION('',(0.,-1.,0.));
#9488=DIRECTION('center_axis',(0.,-1.,0.));
#9489=DIRECTION('ref_axis',(0.,0.,1.));
#9490=DIRECTION('',(0.,-1.,0.));
#9491=DIRECTION('center_axis',(0.,0.,-1.));
#9492=DIRECTION('ref_axis',(-1.,-1.22464679914735E-16,0.));
#9493=DIRECTION('center_axis',(0.,0.,1.));
#9494=DIRECTION('ref_axis',(1.,0.,0.));
#9495=DIRECTION('center_axis',(0.,1.15648231731787E-16,-1.));
#9496=DIRECTION('ref_axis',(0.,1.,1.15648231731787E-16));
#9497=DIRECTION('center_axis',(0.,1.15648231731787E-16,-1.));
#9498=DIRECTION('ref_axis',(0.,1.,1.15648231731787E-16));
#9499=DIRECTION('center_axis',(0.999938130553997,0.,0.0111236263950905));
#9500=DIRECTION('ref_axis',(0.0111236263950905,0.,-0.999938130553997));
#9501=DIRECTION('',(-1.28650731853232E-18,1.,1.15648231731787E-16));
#9502=DIRECTION('center_axis',(0.,0.,1.));
#9503=DIRECTION('ref_axis',(1.,0.,0.));
#9504=DIRECTION('',(-1.,0.,0.));
#9505=DIRECTION('center_axis',(0.,-1.,0.));
#9506=DIRECTION('ref_axis',(-0.0859974399428422,0.,0.996295357975373));
#9507=DIRECTION('',(0.,1.,0.));
#9508=DIRECTION('center_axis',(0.,1.,1.24352412568707E-16));
#9509=DIRECTION('ref_axis',(0.,-1.24352412568707E-16,1.));
#9510=DIRECTION('center_axis',(0.,-1.,-1.24352412568707E-16));
#9511=DIRECTION('ref_axis',(0.,1.24352412568707E-16,-1.));
#9512=DIRECTION('center_axis',(0.,1.,1.24352412568707E-16));
#9513=DIRECTION('ref_axis',(0.,-1.24352412568707E-16,1.));
#9514=DIRECTION('',(0.,1.24352412568707E-16,-1.));
#9515=DIRECTION('',(-1.,0.,0.));
#9516=DIRECTION('center_axis',(0.,-1.,-1.24352412568707E-16));
#9517=DIRECTION('ref_axis',(0.,1.24352412568707E-16,-1.));
#9518=DIRECTION('',(-1.,0.,0.));
#9519=DIRECTION('',(0.,-1.24352412568707E-16,1.));
#9520=DIRECTION('center_axis',(0.,1.15648231731787E-16,-1.));
#9521=DIRECTION('ref_axis',(0.,1.,1.15648231731787E-16));
#9522=DIRECTION('',(0.,-1.,-1.15648231731787E-16));
#9523=DIRECTION('center_axis',(-1.,0.,0.));
#9524=DIRECTION('ref_axis',(0.,0.,1.));
#9525=DIRECTION('center_axis',(1.,0.,-7.88510670898549E-17));
#9526=DIRECTION('ref_axis',(-7.88510670898549E-17,0.,-1.));
#9527=DIRECTION('',(-7.88510670898549E-17,0.,-1.));
#9528=DIRECTION('',(-7.88510670898549E-17,0.,-1.));
#9529=DIRECTION('',(0.,1.,0.));
#9530=DIRECTION('center_axis',(0.,0.,1.));
#9531=DIRECTION('ref_axis',(1.,0.,0.));
#9532=DIRECTION('',(1.,0.,0.));
#9533=DIRECTION('',(0.,1.,0.));
#9534=DIRECTION('',(1.,0.,0.));
#9535=DIRECTION('center_axis',(-1.,0.,1.18276600634782E-16));
#9536=DIRECTION('ref_axis',(1.18276600634782E-16,0.,1.));
#9537=DIRECTION('',(1.18276600634782E-16,0.,1.));
#9538=DIRECTION('',(1.18276600634782E-16,0.,1.));
#9539=DIRECTION('center_axis',(0.,1.,0.));
#9540=DIRECTION('ref_axis',(0.,0.,1.));
#9541=DIRECTION('center_axis',(0.,1.,0.));
#9542=DIRECTION('ref_axis',(0.,0.,1.));
#9543=DIRECTION('axis',(0.,0.,1.));
#9544=DIRECTION('refdir',(1.,0.,0.));
#9545=DIRECTION('center_axis',(0.,-1.,0.));
#9546=DIRECTION('ref_axis',(0.,0.,-1.));
#9547=DIRECTION('center_axis',(0.,-1.,-1.24352412568707E-16));
#9548=DIRECTION('ref_axis',(0.,-1.24352412568707E-16,1.));
#9549=DIRECTION('',(0.,-1.,0.));
#9550=DIRECTION('center_axis',(0.,-1.,0.));
#9551=DIRECTION('ref_axis',(0.,0.,-1.));
#9552=DIRECTION('',(0.,-1.,0.));
#9553=DIRECTION('center_axis',(0.,1.,1.24352412568707E-16));
#9554=DIRECTION('ref_axis',(0.,1.24352412568707E-16,-1.));
#9555=DIRECTION('center_axis',(0.,0.,1.));
#9556=DIRECTION('ref_axis',(1.,0.,0.));
#9557=DIRECTION('center_axis',(0.707106781186583,-1.70853935691577E-13,
0.707106781186512));
#9558=DIRECTION('ref_axis',(0.707106781186512,6.44889800824306E-12,-0.707106781186583));
#9559=DIRECTION('',(0.,0.,1.));
#9560=DIRECTION('center_axis',(-0.707106781186548,0.,0.707106781186548));
#9561=DIRECTION('ref_axis',(0.707106781186547,1.23820750287472E-15,0.707106781186547));
#9562=DIRECTION('',(0.,0.,1.));
#9563=DIRECTION('center_axis',(0.707106781186548,1.36062155274961E-15,-0.707106781186547));
#9564=DIRECTION('ref_axis',(0.707106781186547,-2.36260576158627E-15,0.707106781186548));
#9565=DIRECTION('',(0.,0.,1.));
#9566=DIRECTION('center_axis',(-0.707106781186548,-2.19777105329554E-14,
0.707106781186548));
#9567=DIRECTION('ref_axis',(0.707106781186547,-2.12231778358904E-14,0.707106781186547));
#9568=DIRECTION('',(0.,0.,-1.));
#9569=DIRECTION('center_axis',(0.707106781186576,1.41564689573016E-13,0.707106781186519));
#9570=DIRECTION('ref_axis',(0.707106781186519,3.06847407347585E-11,-0.707106781186576));
#9571=DIRECTION('center_axis',(0.,1.,0.));
#9572=DIRECTION('ref_axis',(0.,0.,1.));
#9573=DIRECTION('center_axis',(0.,-1.,0.));
#9574=DIRECTION('ref_axis',(0.,0.,-1.));
#9575=DIRECTION('',(0.,-1.,0.));
#9576=DIRECTION('center_axis',(0.,1.,0.));
#9577=DIRECTION('ref_axis',(0.,0.,-1.));
#9578=DIRECTION('center_axis',(0.,1.,0.));
#9579=DIRECTION('ref_axis',(0.,0.,1.));
#9580=DIRECTION('center_axis',(0.,-1.,0.));
#9581=DIRECTION('ref_axis',(0.,0.,1.));
#9582=DIRECTION('',(0.,-1.,0.));
#9583=DIRECTION('center_axis',(0.,-1.,0.));
#9584=DIRECTION('ref_axis',(0.,0.,-1.));
#9585=DIRECTION('center_axis',(0.,1.,0.));
#9586=DIRECTION('ref_axis',(0.,0.,1.));
#9587=DIRECTION('center_axis',(0.,-1.,0.));
#9588=DIRECTION('ref_axis',(0.,0.,1.));
#9589=DIRECTION('',(0.,-1.,0.));
#9590=DIRECTION('center_axis',(0.,1.,0.));
#9591=DIRECTION('ref_axis',(0.,0.,-1.));
#9592=DIRECTION('center_axis',(0.,0.,-1.));
#9593=DIRECTION('ref_axis',(-1.,1.20980294963545E-15,0.));
#9594=DIRECTION('center_axis',(0.,0.,1.));
#9595=DIRECTION('ref_axis',(1.,0.,0.));
#9596=DIRECTION('center_axis',(0.,0.,1.));
#9597=DIRECTION('ref_axis',(-1.,0.,0.));
#9598=DIRECTION('center_axis',(0.707106781186548,0.,0.707106781186548));
#9599=DIRECTION('ref_axis',(0.707106781186548,0.,-0.707106781186548));
#9600=DIRECTION('',(-0.707106781186547,0.,0.707106781186547));
#9601=DIRECTION('',(0.,-1.,0.));
#9602=DIRECTION('center_axis',(0.,-1.,0.));
#9603=DIRECTION('ref_axis',(0.,0.,-1.));
#9604=DIRECTION('',(0.707106781186548,0.,0.707106781186548));
#9605=DIRECTION('center_axis',(0.,-1.,0.));
#9606=DIRECTION('ref_axis',(0.,0.,-1.));
#9607=DIRECTION('center_axis',(0.,1.,0.));
#9608=DIRECTION('ref_axis',(0.,0.,1.));
#9609=DIRECTION('',(-0.707106781186547,0.,0.707106781186547));
#9610=DIRECTION('',(-0.707106781186548,0.,-0.707106781186548));
#9611=DIRECTION('center_axis',(0.,1.,0.));
#9612=DIRECTION('ref_axis',(0.,0.,1.));
#9613=DIRECTION('center_axis',(-0.707106781186548,0.,-0.707106781186548));
#9614=DIRECTION('ref_axis',(-0.707106781186548,0.,0.707106781186548));
#9615=DIRECTION('',(-0.707106781186547,0.,0.707106781186547));
#9616=DIRECTION('',(0.,1.,0.));
#9617=DIRECTION('',(-0.707106781186547,0.,0.707106781186547));
#9618=DIRECTION('',(0.,-1.,0.));
#9619=DIRECTION('center_axis',(0.,0.,-1.));
#9620=DIRECTION('ref_axis',(-1.,3.21624529935327E-16,0.));
#9621=DIRECTION('center_axis',(0.,0.,-1.));
#9622=DIRECTION('ref_axis',(1.,1.77635589572802E-15,0.));
#9623=DIRECTION('center_axis',(0.,-1.,0.));
#9624=DIRECTION('ref_axis',(0.,0.,-1.));
#9625=DIRECTION('center_axis',(0.,1.,1.24352412568707E-16));
#9626=DIRECTION('ref_axis',(0.,-1.24352412568707E-16,1.));
#9627=DIRECTION('',(0.,-1.,0.));
#9628=DIRECTION('center_axis',(0.593342281899159,-0.0646221712613811,-0.802352111913568));
#9629=DIRECTION('ref_axis',(-0.738289860535889,-0.440860457545454,-0.510460712300869));
#9630=DIRECTION('',(0.,-1.,0.));
#9631=DIRECTION('center_axis',(0.,-1.,-1.24352412568707E-16));
#9632=DIRECTION('ref_axis',(0.,1.24352412568707E-16,-1.));
#9633=DIRECTION('',(0.,1.,0.));
#9634=DIRECTION('center_axis',(0.999938130553997,0.,0.0111236263950905));
#9635=DIRECTION('ref_axis',(0.0111236263950905,0.,-0.999938130553997));
#9636=DIRECTION('',(0.,-1.,0.));
#9637=DIRECTION('',(0.,1.,0.));
#9638=DIRECTION('center_axis',(0.,0.,1.));
#9639=DIRECTION('ref_axis',(1.,0.,0.));
#9640=DIRECTION('center_axis',(0.,1.,1.24352412568707E-16));
#9641=DIRECTION('ref_axis',(0.,-1.24352412568707E-16,1.));
#9642=DIRECTION('center_axis',(0.,1.,1.24352412568707E-16));
#9643=DIRECTION('ref_axis',(0.,-1.24352412568707E-16,1.));
#9644=DIRECTION('center_axis',(0.,1.,1.24352412568707E-16));
#9645=DIRECTION('ref_axis',(0.,-1.24352412568707E-16,1.));
#9646=DIRECTION('',(0.,1.24352412568707E-16,-1.));
#9647=DIRECTION('',(-1.,0.,0.));
#9648=DIRECTION('',(0.,1.15648231731787E-16,-1.));
#9649=DIRECTION('center_axis',(0.,-1.,-1.24352412568707E-16));
#9650=DIRECTION('ref_axis',(0.,1.24352412568707E-16,-1.));
#9651=DIRECTION('center_axis',(0.,-1.,-1.24352412568707E-16));
#9652=DIRECTION('ref_axis',(0.,1.24352412568707E-16,-1.));
#9653=DIRECTION('center_axis',(0.,-1.,-1.24352412568707E-16));
#9654=DIRECTION('ref_axis',(0.,1.24352412568707E-16,-1.));
#9655=DIRECTION('',(0.,1.15648231731787E-16,-1.));
#9656=DIRECTION('',(1.,-2.15636651137065E-16,0.));
#9657=DIRECTION('',(0.,-1.24352412568707E-16,1.));
#9658=DIRECTION('center_axis',(-1.,0.,0.));
#9659=DIRECTION('ref_axis',(0.,0.,1.));
#9660=DIRECTION('',(0.,1.,2.10269512239613E-16));
#9661=DIRECTION('center_axis',(0.,0.,1.));
#9662=DIRECTION('ref_axis',(1.,0.,0.));
#9663=DIRECTION('center_axis',(0.,0.,-1.));
#9664=DIRECTION('ref_axis',(1.,0.,0.));
#9665=DIRECTION('',(-1.,0.,0.));
#9666=DIRECTION('',(0.,1.,0.));
#9667=DIRECTION('',(-1.,0.,0.));
#9668=DIRECTION('center_axis',(0.,-1.,0.));
#9669=DIRECTION('ref_axis',(0.,0.,-1.));
#9670=DIRECTION('',(0.707106781186547,0.,-0.707106781186547));
#9671=DIRECTION('center_axis',(0.,1.,0.));
#9672=DIRECTION('ref_axis',(0.,0.,-1.));
#9673=DIRECTION('',(0.707106781186548,0.,0.707106781186548));
#9674=DIRECTION('',(-1.,0.,0.));
#9675=DIRECTION('',(0.707106781186548,0.,0.707106781186548));
#9676=DIRECTION('center_axis',(0.,1.,0.));
#9677=DIRECTION('ref_axis',(3.15404268359419E-15,0.,-1.));
#9678=DIRECTION('center_axis',(0.,0.,-1.));
#9679=DIRECTION('ref_axis',(-1.,0.,0.));
#9680=DIRECTION('',(0.,-1.,0.));
#9681=DIRECTION('',(-1.,0.,0.));
#9682=DIRECTION('center_axis',(0.,1.,0.));
#9683=DIRECTION('ref_axis',(0.,0.,1.));
#9684=DIRECTION('',(0.707106781186548,0.,0.707106781186548));
#9685=DIRECTION('center_axis',(0.,-1.,0.));
#9686=DIRECTION('ref_axis',(3.15404268359419E-15,0.,1.));
#9687=DIRECTION('center_axis',(0.,-1.,0.));
#9688=DIRECTION('ref_axis',(-3.15404268359419E-15,0.,1.));
#9689=DIRECTION('',(0.707106781186548,0.,0.707106781186548));
#9690=DIRECTION('',(-0.0186217163628307,0.,-0.999826600806211));
#9691=DIRECTION('center_axis',(0.,0.,-1.));
#9692=DIRECTION('ref_axis',(1.,0.,0.));
#9693=DIRECTION('center_axis',(-0.707106781186548,0.,0.707106781186547));
#9694=DIRECTION('ref_axis',(0.707106781186547,0.,0.707106781186548));
#9695=DIRECTION('',(-0.707106781186548,0.,-0.707106781186548));
#9696=DIRECTION('',(0.,1.,0.));
#9697=DIRECTION('',(0.,1.,0.));
#9698=DIRECTION('',(0.707106781186548,0.,0.707106781186548));
#9699=DIRECTION('',(0.,1.,0.));
#9700=DIRECTION('center_axis',(0.707106781186548,0.,-0.707106781186547));
#9701=DIRECTION('ref_axis',(-0.707106781186547,0.,-0.707106781186548));
#9702=DIRECTION('',(-0.707106781186548,0.,-0.707106781186548));
#9703=DIRECTION('',(0.707106781186548,0.,0.707106781186548));
#9704=DIRECTION('',(0.,-1.,0.));
#9705=DIRECTION('',(0.,-1.,0.));
#9706=DIRECTION('center_axis',(-0.707106781186548,0.,-0.707106781186548));
#9707=DIRECTION('ref_axis',(-0.707106781186548,0.,0.707106781186548));
#9708=DIRECTION('',(0.707106781186547,0.,-0.707106781186547));
#9709=DIRECTION('',(0.,1.,0.));
#9710=DIRECTION('',(0.,-1.,0.));
#9711=DIRECTION('center_axis',(0.707106781186548,0.,0.707106781186548));
#9712=DIRECTION('ref_axis',(0.707106781186548,0.,-0.707106781186548));
#9713=DIRECTION('',(0.,-1.,0.));
#9714=DIRECTION('center_axis',(0.,-1.,0.));
#9715=DIRECTION('ref_axis',(0.,0.,-1.));
#9716=DIRECTION('center_axis',(0.,1.,0.));
#9717=DIRECTION('ref_axis',(-6.30808536718839E-15,0.,-1.));
#9718=DIRECTION('center_axis',(0.,1.,0.));
#9719=DIRECTION('ref_axis',(-3.1540426835942E-15,0.,-1.));
#9720=DIRECTION('center_axis',(0.,1.,0.));
#9721=DIRECTION('ref_axis',(0.,0.,1.));
#9722=DIRECTION('center_axis',(0.,-1.,0.));
#9723=DIRECTION('ref_axis',(0.,0.,1.));
#9724=DIRECTION('center_axis',(0.,-1.,0.));
#9725=DIRECTION('ref_axis',(-3.15404268359419E-15,0.,1.));
#9726=DIRECTION('center_axis',(0.,-1.,0.));
#9727=DIRECTION('ref_axis',(0.,0.,-1.));
#9728=DIRECTION('center_axis',(0.,-1.,0.));
#9729=DIRECTION('ref_axis',(0.,0.,-1.));
#9730=DIRECTION('center_axis',(0.,-1.,0.));
#9731=DIRECTION('ref_axis',(0.,0.,-1.));
#9732=DIRECTION('center_axis',(0.,-1.,0.));
#9733=DIRECTION('ref_axis',(0.,0.,-1.));
#9734=DIRECTION('center_axis',(0.,1.,0.));
#9735=DIRECTION('ref_axis',(2.78699993901511E-15,0.,-1.));
#9736=DIRECTION('center_axis',(0.,1.,0.));
#9737=DIRECTION('ref_axis',(2.78699993901511E-15,0.,-1.));
#9738=DIRECTION('center_axis',(0.,1.,0.));
#9739=DIRECTION('ref_axis',(-1.89882151931499E-15,0.,-1.));
#9740=DIRECTION('center_axis',(0.,1.,0.));
#9741=DIRECTION('ref_axis',(0.,0.,1.));
#9742=DIRECTION('',(0.,1.,0.));
#9743=DIRECTION('',(0.,1.,0.));
#9744=DIRECTION('',(0.,1.,0.));
#9745=DIRECTION('center_axis',(1.,0.,0.));
#9746=DIRECTION('ref_axis',(0.,0.,-1.));
#9747=DIRECTION('',(0.,-1.,-2.10269512239613E-16));
#9748=DIRECTION('center_axis',(4.53418134555742E-32,2.10269512239613E-16,
-1.));
#9749=DIRECTION('ref_axis',(0.,1.,2.10269512239613E-16));
#9750=DIRECTION('center_axis',(0.,1.,0.));
#9751=DIRECTION('ref_axis',(0.,0.,1.));
#9752=DIRECTION('center_axis',(0.,1.,0.));
#9753=DIRECTION('ref_axis',(0.,0.,1.));
#9754=DIRECTION('axis',(0.,0.,1.));
#9755=DIRECTION('refdir',(1.,0.,0.));
#9756=DIRECTION('center_axis',(0.,-1.,0.));
#9757=DIRECTION('ref_axis',(0.,0.,-1.));
#9758=DIRECTION('center_axis',(-1.,0.,-1.22464679914735E-16));
#9759=DIRECTION('ref_axis',(-1.22464679914735E-16,0.,1.));
#9760=DIRECTION('center_axis',(0.,-1.,0.));
#9761=DIRECTION('ref_axis',(0.,0.,-1.));
#9762=DIRECTION('center_axis',(-1.,0.,-1.22464679914735E-16));
#9763=DIRECTION('ref_axis',(-1.22464679914735E-16,0.,1.));
#9764=DIRECTION('center_axis',(0.,-1.,0.));
#9765=DIRECTION('ref_axis',(0.,0.,-1.));
#9766=DIRECTION('axis',(0.,0.,1.));
#9767=DIRECTION('refdir',(1.,0.,0.));
#9768=DIRECTION('axis',(0.,0.,1.));
#9769=DIRECTION('refdir',(1.,0.,0.));
#9770=DIRECTION('center_axis',(0.,0.,1.));
#9771=DIRECTION('ref_axis',(1.,0.,0.));
#9772=DIRECTION('center_axis',(0.,0.,1.));
#9773=DIRECTION('ref_axis',(1.,0.,0.));
#9774=DIRECTION('',(0.,0.,1.));
#9775=DIRECTION('center_axis',(0.,0.,1.));
#9776=DIRECTION('ref_axis',(1.,0.,0.));
#9777=DIRECTION('center_axis',(1.,-1.0842021724855E-16,0.));
#9778=DIRECTION('ref_axis',(1.0842021724855E-16,1.,0.));
#9779=DIRECTION('center_axis',(1.,-7.2280144832367E-17,0.));
#9780=DIRECTION('ref_axis',(7.2280144832367E-17,1.,0.));
#9781=DIRECTION('',(1.,-1.0842021724855E-16,0.));
#9782=DIRECTION('center_axis',(1.,-1.0842021724855E-16,0.));
#9783=DIRECTION('ref_axis',(1.0842021724855E-16,1.,0.));
#9784=DIRECTION('center_axis',(0.,0.,-1.));
#9785=DIRECTION('ref_axis',(-1.,0.,0.));
#9786=DIRECTION('center_axis',(0.,0.,1.));
#9787=DIRECTION('ref_axis',(1.,0.,0.));
#9788=DIRECTION('',(0.,0.,1.));
#9789=DIRECTION('center_axis',(0.,0.,1.));
#9790=DIRECTION('ref_axis',(1.,0.,0.));
#9791=DIRECTION('center_axis',(0.,0.,1.));
#9792=DIRECTION('ref_axis',(1.,0.,0.));
#9793=DIRECTION('',(7.2280144832367E-17,1.,0.));
#9794=DIRECTION('',(-1.,0.,0.));
#9795=DIRECTION('',(-1.44560289664734E-16,-1.,0.));
#9796=DIRECTION('',(1.,0.,0.));
#9797=DIRECTION('center_axis',(0.,0.,1.));
#9798=DIRECTION('ref_axis',(1.,0.,0.));
#9799=DIRECTION('center_axis',(1.,-7.2280144832367E-17,0.));
#9800=DIRECTION('ref_axis',(7.2280144832367E-17,1.,0.));
#9801=DIRECTION('center_axis',(-1.,7.2280144832367E-17,0.));
#9802=DIRECTION('ref_axis',(7.2280144832367E-17,1.,0.));
#9803=DIRECTION('',(0.,0.,1.));
#9804=DIRECTION('',(0.,0.,1.));
#9805=DIRECTION('center_axis',(0.,-1.,0.));
#9806=DIRECTION('ref_axis',(0.,0.,-1.));
#9807=DIRECTION('',(0.,0.,1.));
#9808=DIRECTION('',(-1.,0.,0.));
#9809=DIRECTION('center_axis',(-1.,1.44560289664734E-16,0.));
#9810=DIRECTION('ref_axis',(-1.44560289664734E-16,-1.,0.));
#9811=DIRECTION('',(0.,0.,1.));
#9812=DIRECTION('center_axis',(1.,-1.44560289664734E-16,0.));
#9813=DIRECTION('ref_axis',(-1.44560289664734E-16,-1.,0.));
#9814=DIRECTION('center_axis',(0.,1.,0.));
#9815=DIRECTION('ref_axis',(0.,0.,1.));
#9816=DIRECTION('',(1.,0.,0.));
#9817=DIRECTION('center_axis',(-1.,0.,0.));
#9818=DIRECTION('ref_axis',(0.,1.22464679914735E-16,-1.));
#9819=DIRECTION('center_axis',(0.,0.,1.));
#9820=DIRECTION('ref_axis',(1.,0.,0.));
#9821=DIRECTION('axis',(0.,0.,1.));
#9822=DIRECTION('refdir',(1.,0.,0.));
#9823=DIRECTION('center_axis',(1.,1.23908819712629E-16,0.));
#9824=DIRECTION('ref_axis',(-1.23908819712629E-16,1.,0.));
#9825=DIRECTION('center_axis',(1.,1.23908819712629E-16,0.));
#9826=DIRECTION('ref_axis',(-1.23908819712629E-16,1.,0.));
#9827=DIRECTION('',(1.,1.23908819712629E-16,0.));
#9828=DIRECTION('center_axis',(1.,1.23908819712629E-16,0.));
#9829=DIRECTION('ref_axis',(-1.23908819712629E-16,1.,0.));
#9830=DIRECTION('center_axis',(1.,1.23908819712629E-16,0.));
#9831=DIRECTION('ref_axis',(1.92592994438723E-32,-1.60812264967664E-16,
1.));
#9832=DIRECTION('center_axis',(-1.,-1.23908819712629E-16,0.));
#9833=DIRECTION('ref_axis',(-1.23908819712629E-16,1.,0.));
#9834=DIRECTION('',(-1.,-1.23908819712629E-16,0.));
#9835=DIRECTION('center_axis',(1.,1.23908819712629E-16,0.));
#9836=DIRECTION('ref_axis',(-1.23908819712629E-16,1.,0.));
#9837=DIRECTION('',(1.,1.23908819712629E-16,0.));
#9838=DIRECTION('center_axis',(0.,0.,-1.));
#9839=DIRECTION('ref_axis',(-1.,0.,0.));
#9840=DIRECTION('center_axis',(0.,0.,1.));
#9841=DIRECTION('ref_axis',(1.,0.,0.));
#9842=DIRECTION('',(0.,0.,1.));
#9843=DIRECTION('center_axis',(0.,0.,1.));
#9844=DIRECTION('ref_axis',(1.,0.,0.));
#9845=DIRECTION('center_axis',(0.,0.,1.));
#9846=DIRECTION('ref_axis',(1.,0.,0.));
#9847=DIRECTION('',(-1.,0.,0.));
#9848=DIRECTION('',(-1.23908819712629E-16,1.,0.));
#9849=DIRECTION('',(1.,0.,0.));
#9850=DIRECTION('',(1.23908819712629E-16,-1.,0.));
#9851=DIRECTION('center_axis',(0.,0.,1.));
#9852=DIRECTION('ref_axis',(1.,0.,0.));
#9853=DIRECTION('center_axis',(-1.,-1.23908819712629E-16,0.));
#9854=DIRECTION('ref_axis',(1.23908819712629E-16,-1.,0.));
#9855=DIRECTION('',(0.,0.,-1.));
#9856=DIRECTION('',(0.,0.,-1.));
#9857=DIRECTION('center_axis',(0.,-1.,0.));
#9858=DIRECTION('ref_axis',(0.,0.,-1.));
#9859=DIRECTION('',(0.,0.,-1.));
#9860=DIRECTION('center_axis',(1.,1.23908819712629E-16,0.));
#9861=DIRECTION('ref_axis',(-1.23908819712629E-16,1.,0.));
#9862=DIRECTION('',(0.,0.,-1.));
#9863=DIRECTION('center_axis',(0.,1.,0.));
#9864=DIRECTION('ref_axis',(0.,0.,1.));
#9865=DIRECTION('',(2.08166817117217E-17,-2.22044604925031E-16,1.));
#9866=DIRECTION('',(1.,5.55111512312579E-17,-2.08166817117217E-17));
#9867=DIRECTION('',(2.08166817117217E-17,-2.22044604925031E-16,1.));
#9868=DIRECTION('',(1.,5.55111512312579E-17,-2.08166817117217E-17));
#9869=DIRECTION('',(1.38777878078145E-17,1.38777878078145E-17,1.));
#9870=DIRECTION('',(1.,1.11022302462516E-16,-1.38777878078145E-17));
#9871=DIRECTION('',(-1.,-5.55111512312578E-17,9.71445146547012E-17));
#9872=DIRECTION('',(3.22356430262057E-17,-0.974370064785235,-0.224951054343865));
#9873=DIRECTION('',(-0.56106925706888,-0.806553199620807,-0.18620747824299));
#9874=DIRECTION('',(0.827768861924737,-0.546689088359208,-0.126213120937574));
#9875=DIRECTION('',(0.436387525769707,-0.0970541721281935,-0.894509035742571));
#9876=DIRECTION('',(0.703396912222942,-0.58314014083576,0.406423867435565));
#9877=DIRECTION('',(-0.999995451424921,0.00293884120638094,0.0006784849533224));
#9878=DIRECTION('',(-3.26874775999101E-17,-0.224951054343865,0.974370064785235));
#9879=DIRECTION('',(1.,1.13269149580016E-16,5.55111512312578E-17));
#9880=DIRECTION('',(5.55111512312578E-17,-4.65585392816269E-17,-1.));
#9881=DIRECTION('',(-0.647908751826441,0.761717959159887,-3.43123515092284E-18));
#9882=DIRECTION('',(-0.761717959159887,-0.647908751826441,-5.55111512312578E-16));
#9883=DIRECTION('',(-0.258819045102518,-0.961399932042652,0.0933963198450862));
#9884=DIRECTION('',(0.737690728744535,-0.259156837416095,-0.62341809593951));
#9885=CARTESIAN_POINT('',(0.,0.,0.));
#9886=CARTESIAN_POINT('',(0.,0.,0.));
#9887=CARTESIAN_POINT('Origin',(-3.28761363381793,19.7279394918662,23.));
#9888=CARTESIAN_POINT('',(13.5840213174672,33.8470022819586,25.));
#9889=CARTESIAN_POINT('',(0.522929774013513,-1.9395421093036,25.));
#9890=CARTESIAN_POINT('Origin',(-3.28761363381793,19.7279394918662,25.));
#9891=CARTESIAN_POINT('',(12.0502363218959,32.563451119223,23.));
#9892=CARTESIAN_POINT('Origin',(13.5840213174673,33.8470022819586,23.));
#9893=CARTESIAN_POINT('',(0.176516736937927,0.0302289453482035,23.));
#9894=CARTESIAN_POINT('Origin',(-3.28761363381793,19.7279394918662,23.));
#9895=CARTESIAN_POINT('Origin',(0.522929774013513,-1.9395421093036,23.));
#9896=CARTESIAN_POINT('Origin',(-3.28761363381793,19.7279394918662,2.));
#9897=CARTESIAN_POINT('',(12.0502363218959,32.563451119223,2.));
#9898=CARTESIAN_POINT('',(0.176516736937927,0.0302289453482035,2.));
#9899=CARTESIAN_POINT('Origin',(-3.28761363381793,19.7279394918662,2.));
#9900=CARTESIAN_POINT('',(13.5840213174673,33.8470022819586,0.));
#9901=CARTESIAN_POINT('Origin',(13.5840213174672,33.8470022819586,2.));
#9902=CARTESIAN_POINT('',(0.522929774013513,-1.9395421093036,0.));
#9903=CARTESIAN_POINT('Origin',(-3.28761363381793,19.7279394918662,0.));
#9904=CARTESIAN_POINT('Origin',(0.522929774013513,-1.9395421093036,2.));
#9905=CARTESIAN_POINT('Origin',(30.,84.6000761633705,2.));
#9906=CARTESIAN_POINT('',(32.,84.6000761633705,2.));
#9907=CARTESIAN_POINT('',(29.7519485792559,86.5846341727688,2.));
#9908=CARTESIAN_POINT('Origin',(30.,84.6000761633705,2.));
#9909=CARTESIAN_POINT('',(30.,84.6000761633705,0.));
#9910=CARTESIAN_POINT('Origin',(30.,84.6000761633705,2.));
#9911=CARTESIAN_POINT('Origin',(30.,84.6000761633705,2.));
#9912=CARTESIAN_POINT('Origin',(-3.32467333292967,13.7193061680048,10.8273365655636));
#9913=CARTESIAN_POINT('',(-3.05145636383197,16.9216708811215,10.136042009416));
#9914=CARTESIAN_POINT('Origin',(-3.05145636383197,16.5317379207667,11.5844729834113));
#9915=CARTESIAN_POINT('',(-2.39071013447879,23.7232384487861,11.9670960425935));
#9916=CARTESIAN_POINT('',(-3.32467333292967,14.1092391283596,9.37890559156828));
#9917=CARTESIAN_POINT('Origin',(-2.39071013447879,23.3333054884313,13.4155270165888));
#9918=CARTESIAN_POINT('Origin',(26.0000000000001,96.3501340213216,12.5));
#9919=CARTESIAN_POINT('',(23.,96.3501340213216,11.));
#9920=CARTESIAN_POINT('Origin',(23.,96.3501340213216,12.5));
#9921=CARTESIAN_POINT('',(8.00000000000006,96.3501340213216,11.));
#9922=CARTESIAN_POINT('',(26.0000000000001,96.3501340213216,11.));
#9923=CARTESIAN_POINT('Origin',(8.00000000000006,96.3501340213216,12.5));
#9924=CARTESIAN_POINT('Origin',(55.3717972015101,68.8171894196414,25.));
#9925=CARTESIAN_POINT('',(-0.227371959941596,78.8083638429823,23.));
#9926=CARTESIAN_POINT('Origin',(55.3717972015101,68.8171894196414,23.));
#9927=CARTESIAN_POINT('',(-0.227371959941596,78.8083638429823,2.));
#9928=CARTESIAN_POINT('',(-0.227371959941595,78.8083638429823,25.));
#9929=CARTESIAN_POINT('Origin',(55.3717972015101,68.8171894196414,2.));
#9930=CARTESIAN_POINT('',(12.0502363218959,32.563451119223,25.));
#9931=CARTESIAN_POINT('Origin',(-7.93301877845108,21.7616127890893,21.2536537832198));
#9932=CARTESIAN_POINT('',(11.9915524290357,19.8260170362199,21.2536537832198));
#9933=CARTESIAN_POINT('',(16.7091421738371,19.3677212677073,21.2536537832198));
#9934=CARTESIAN_POINT('',(-7.93301877845108,21.7616127890893,21.2536537832198));
#9935=CARTESIAN_POINT('',(11.3308061996825,13.0244494685553,19.4225997500424));
#9936=CARTESIAN_POINT('',(11.9915524290357,19.8260170362198,21.2536537832198));
#9937=CARTESIAN_POINT('',(15.409807546716,12.6281901161683,19.4225997500424));
#9938=CARTESIAN_POINT('',(-8.59376500780425,14.9600452214247,19.4225997500424));
#9939=CARTESIAN_POINT('Origin',(-3.28761363374331,19.7279394918536,20.831640338319));
#9940=CARTESIAN_POINT('Origin',(-7.52687414707159,25.9423708923569,5.57740024995768));
#9941=CARTESIAN_POINT('',(12.0795247373973,24.0376843616083,5.57740024995768));
#9942=CARTESIAN_POINT('',(16.3290636231184,23.6248579407434,5.57740024995768));
#9943=CARTESIAN_POINT('',(-7.52687414707159,25.9423708923569,5.57740024995768));
#9944=CARTESIAN_POINT('',(2.79035956011326,24.4747961873976,7.30576827714592));
#9945=CARTESIAN_POINT('Origin',(11.453888025434,17.5975259767542,29.7255459071844));
#9946=CARTESIAN_POINT('',(-2.39071013447879,24.4418545686223,9.2977504057545));
#9947=CARTESIAN_POINT('',(2.67091952913043,24.4740367789744,7.3516897607744));
#9948=CARTESIAN_POINT('',(-2.39071013447879,22.2247564082402,17.533303627423));
#9949=CARTESIAN_POINT('Origin',(-0.814358709812287,23.1905174560636,13.3770869658276));
#9950=CARTESIAN_POINT('',(2.94819571840111,21.1535027599203,19.5859695192486));
#9951=CARTESIAN_POINT('',(-2.29893826609133,22.206342345222,17.5685874457294));
#9952=CARTESIAN_POINT('Origin',(12.6171891409989,26.266175421074,-2.89449187400689));
#9953=CARTESIAN_POINT('Origin',(-3.28761363568232,19.7279394916906,27.1315428110125));
#9954=CARTESIAN_POINT('Origin',(-7.52687414707159,25.9423708923569,5.57740024995768));
#9955=CARTESIAN_POINT('',(11.4187785080441,17.2361167939437,3.74634621678022));
#9956=CARTESIAN_POINT('',(16.4884781618741,16.7436148968595,3.74634621678022));
#9957=CARTESIAN_POINT('',(-8.18762037642477,19.1408033246923,3.74634621678022));
#9958=CARTESIAN_POINT('',(12.0795247373973,24.0376843616084,5.57740024995771));
#9959=CARTESIAN_POINT('Origin',(-3.28761363374728,19.7279394918659,4.02988243998975));
#9960=CARTESIAN_POINT('Origin',(-8.18762037642477,19.1408033246923,3.74634621678022));
#9961=CARTESIAN_POINT('',(2.12961333076012,17.673228619733,5.47471424396846));
#9962=CARTESIAN_POINT('',(-3.05145636383197,17.6402870009577,7.46669637257706));
#9963=CARTESIAN_POINT('',(2.01017329977726,17.6724692113098,5.52063572759696));
#9964=CARTESIAN_POINT('Origin',(10.7931417960809,10.7959584090896,27.8944918740069));
#9965=CARTESIAN_POINT('Origin',(-3.28761363445173,19.7279394920272,-0.202803923569845));
#9966=CARTESIAN_POINT('',(2.2874494890479,14.3519351922557,17.7549154860712));
#9967=CARTESIAN_POINT('Origin',(11.9564429116457,19.4646078534094,-4.72554590718435));
#9968=CARTESIAN_POINT('',(-3.05145636383196,15.4231888405756,15.7022495942456));
#9969=CARTESIAN_POINT('',(-2.95968449544451,15.4047747775574,15.737533412552));
#9970=CARTESIAN_POINT('Origin',(-1.47510493916546,16.388949888399,11.5460329326502));
#9971=CARTESIAN_POINT('Origin',(50.,-75.4117474694202,25.));
#9972=CARTESIAN_POINT('',(1.14256307744359,80.3629684149532,23.));
#9973=CARTESIAN_POINT('',(29.7519485792559,86.5846341727688,23.));
#9974=CARTESIAN_POINT('Origin',(50.,-75.4117474694202,23.));
#9975=CARTESIAN_POINT('',(29.7519485792559,86.5846341727688,25.));
#9976=CARTESIAN_POINT('',(1.14256307744359,80.3629684149532,2.));
#9977=CARTESIAN_POINT('Origin',(50.,-75.4117474694202,2.));
#9978=CARTESIAN_POINT('',(1.14256307744358,80.3629684149533,25.));
#9979=CARTESIAN_POINT('',(23.,85.5969828885913,7.5));
#9980=CARTESIAN_POINT('',(23.,85.5969828885913,22.5));
#9981=CARTESIAN_POINT('',(23.,85.5969828885913,25.));
#9982=CARTESIAN_POINT('',(8.00000000000003,82.3501340213215,22.5));
#9983=CARTESIAN_POINT('Origin',(50.,-75.4117474694202,22.5));
#9984=CARTESIAN_POINT('',(8.00000000000004,82.3501340213216,7.5));
#9985=CARTESIAN_POINT('',(8.00000000000004,82.3501340213216,7.5));
#9986=CARTESIAN_POINT('Origin',(50.,-75.4117474694202,7.5));
#9987=CARTESIAN_POINT('Origin',(0.,0.,17.5));
#9988=CARTESIAN_POINT('',(8.00000000000003,90.0969828885913,17.5));
#9989=CARTESIAN_POINT('',(8.00000000000003,101.350134021322,17.5));
#9990=CARTESIAN_POINT('',(8.00000000000006,2.19122965386546E-15,17.5));
#9991=CARTESIAN_POINT('',(23.,90.0969828885913,17.5));
#9992=CARTESIAN_POINT('',(8.00000000000004,90.0969828885913,17.5));
#9993=CARTESIAN_POINT('',(23.,101.350134021322,17.5));
#9994=CARTESIAN_POINT('',(23.,0.,17.5));
#9995=CARTESIAN_POINT('',(0.,101.350134021322,17.5));
#9996=CARTESIAN_POINT('Origin',(-3.28761363381793,19.7279394918662,25.));
#9997=CARTESIAN_POINT('',(0.176516736937928,0.0302289453482027,25.));
#9998=CARTESIAN_POINT('Origin',(0.,0.,25.));
#9999=CARTESIAN_POINT('',(-18.,-2.20436423846524E-15,23.));
#10000=CARTESIAN_POINT('',(-0.169896300137657,-2.0806296015056E-17,23.));
#10001=CARTESIAN_POINT('',(1.88751509164731E-16,2.3115393153282E-32,23.));
#10002=CARTESIAN_POINT('',(-0.169896300137657,-2.0806296015056E-17,2.));
#10003=CARTESIAN_POINT('',(-0.169896300137657,-2.0806296015056E-17,0.));
#10004=CARTESIAN_POINT('',(-18.,-2.20436423846524E-15,2.));
#10005=CARTESIAN_POINT('',(0.,0.,2.));
#10006=CARTESIAN_POINT('',(-18.,-2.20436423846524E-15,25.));
#10007=CARTESIAN_POINT('Origin',(-20.,-2.44929359829471E-15,25.));
#10008=CARTESIAN_POINT('',(-20.,-13.,23.));
#10009=CARTESIAN_POINT('',(-20.,-2.,23.));
#10010=CARTESIAN_POINT('',(-20.,-3.93203987888076E-15,23.));
#10011=CARTESIAN_POINT('',(-20.,-2.,2.));
#10012=CARTESIAN_POINT('',(-20.,-2.,25.));
#10013=CARTESIAN_POINT('',(-20.,-13.,2.));
#10014=CARTESIAN_POINT('',(-20.,-2.44929359829471E-15,2.));
#10015=CARTESIAN_POINT('',(-20.,-13.,25.));
#10016=CARTESIAN_POINT('Origin',(-20.,-15.,25.));
#10017=CARTESIAN_POINT('',(30.,-15.,23.));
#10018=CARTESIAN_POINT('',(-18.,-15.,23.));
#10019=CARTESIAN_POINT('',(-20.,-15.,23.));
#10020=CARTESIAN_POINT('',(-18.,-15.,2.));
#10021=CARTESIAN_POINT('',(-18.,-15.,25.));
#10022=CARTESIAN_POINT('',(30.,-15.,2.));
#10023=CARTESIAN_POINT('',(-20.,-15.,2.));
#10024=CARTESIAN_POINT('',(30.,-15.,25.));
#10025=CARTESIAN_POINT('Origin',(32.,86.8498045122456,25.));
#10026=CARTESIAN_POINT('',(32.,84.6000761633705,23.));
#10027=CARTESIAN_POINT('',(32.,-13.,23.));
#10028=CARTESIAN_POINT('',(32.,-15.,23.));
#10029=CARTESIAN_POINT('',(32.,-13.,2.));
#10030=CARTESIAN_POINT('',(32.,-13.,25.));
#10031=CARTESIAN_POINT('',(32.,86.8498045122456,2.));
#10032=CARTESIAN_POINT('',(32.,84.6000761633705,25.));
#10033=CARTESIAN_POINT('Origin',(-3.28761363381793,19.7279394918662,25.));
#10034=CARTESIAN_POINT('',(30.,84.6000761633705,25.));
#10035=CARTESIAN_POINT('',(1.74109754333981,78.4546297413593,25.));
#10036=CARTESIAN_POINT('Origin',(50.,-75.4117474694202,25.));
#10037=CARTESIAN_POINT('Origin',(55.3717972015101,68.8171894196414,25.));
#10038=CARTESIAN_POINT('',(-0.169896300137657,-2.,25.));
#10039=CARTESIAN_POINT('Origin',(-0.169896300137657,2.,25.));
#10040=CARTESIAN_POINT('',(-18.,-2.,25.));
#10041=CARTESIAN_POINT('',(-20.,-2.,25.));
#10042=CARTESIAN_POINT('',(-18.,-13.,25.));
#10043=CARTESIAN_POINT('',(-18.,-15.,25.));
#10044=CARTESIAN_POINT('',(30.,-13.,25.));
#10045=CARTESIAN_POINT('',(32.,-13.,25.));
#10046=CARTESIAN_POINT('',(30.,86.8498045122456,25.));
#10047=CARTESIAN_POINT('Origin',(-3.28761363381793,19.7279394918662,0.));
#10048=CARTESIAN_POINT('',(-0.169896300137657,-2.,0.));
#10049=CARTESIAN_POINT('Origin',(-0.169896300137657,2.,0.));
#10050=CARTESIAN_POINT('',(1.74109754333981,78.4546297413593,0.));
#10051=CARTESIAN_POINT('Origin',(55.3717972015101,68.8171894196414,0.));
#10052=CARTESIAN_POINT('Origin',(50.,-75.4117474694202,0.));
#10053=CARTESIAN_POINT('',(30.,-13.,0.));
#10054=CARTESIAN_POINT('',(30.,19.7279394918662,0.));
#10055=CARTESIAN_POINT('',(-18.,-13.,0.));
#10056=CARTESIAN_POINT('',(-3.28761363381793,-13.,0.));
#10057=CARTESIAN_POINT('',(-18.,-2.,0.));
#10058=CARTESIAN_POINT('',(-18.,19.7279394918662,0.));
#10059=CARTESIAN_POINT('',(-3.28761363381793,-2.,0.));
#10060=CARTESIAN_POINT('Origin',(23.,0.,7.5));
#10061=CARTESIAN_POINT('',(23.,93.3501340213216,7.5));
#10062=CARTESIAN_POINT('',(23.,0.,7.5));
#10063=CARTESIAN_POINT('',(23.,101.350134021322,15.5));
#10064=CARTESIAN_POINT('Origin',(23.,93.3501340213216,15.5));
#10065=CARTESIAN_POINT('',(23.,101.350134021322,7.5));
#10066=CARTESIAN_POINT('',(23.,90.0969828885913,22.5));
#10067=CARTESIAN_POINT('',(23.,90.0969828885913,22.5));
#10068=CARTESIAN_POINT('',(23.,85.5969828885913,22.5));
#10069=CARTESIAN_POINT('Origin',(8.00000000000006,2.19122965386546E-15,
7.5));
#10070=CARTESIAN_POINT('',(8.00000000000003,101.350134021322,15.5));
#10071=CARTESIAN_POINT('',(8.00000000000003,101.350134021322,7.5));
#10072=CARTESIAN_POINT('',(8.00000000000003,93.3501340213216,7.5));
#10073=CARTESIAN_POINT('Origin',(8.00000000000003,93.3501340213216,15.5));
#10074=CARTESIAN_POINT('',(8.00000000000006,2.19122965386546E-15,7.5));
#10075=CARTESIAN_POINT('',(8.00000000000004,90.0969828885913,22.5));
#10076=CARTESIAN_POINT('',(8.00000000000003,82.3501340213215,22.5));
#10077=CARTESIAN_POINT('',(8.00000000000004,90.0969828885913,22.5));
#10078=CARTESIAN_POINT('Origin',(0.,101.350134021322,7.5));
#10079=CARTESIAN_POINT('',(0.,101.350134021322,15.5));
#10080=CARTESIAN_POINT('Origin',(0.,0.,7.5));
#10081=CARTESIAN_POINT('',(0.,93.3501340213216,7.5));
#10082=CARTESIAN_POINT('Origin',(0.,93.3501340213216,15.5));
#10083=CARTESIAN_POINT('Origin',(8.00000000000004,90.0969828885913,22.5));
#10084=CARTESIAN_POINT('',(8.00000000000004,90.0969828885913,22.5));
#10085=CARTESIAN_POINT('Origin',(50.,-75.4117474694202,22.5));
#10086=CARTESIAN_POINT('Origin',(-20.,-13.,2.));
#10087=CARTESIAN_POINT('Origin',(-18.,-13.,2.));
#10088=CARTESIAN_POINT('Origin',(30.,-13.,2.));
#10089=CARTESIAN_POINT('Origin',(-18.,-13.,2.));
#10090=CARTESIAN_POINT('Origin',(-18.,-13.,2.));
#10091=CARTESIAN_POINT('Origin',(-18.,-13.,2.));
#10092=CARTESIAN_POINT('Origin',(30.,-13.,2.));
#10093=CARTESIAN_POINT('Origin',(30.,-13.,2.));
#10094=CARTESIAN_POINT('Origin',(30.,-13.,2.));
#10095=CARTESIAN_POINT('Origin',(-18.,-13.,25.));
#10096=CARTESIAN_POINT('Origin',(-18.,-13.,23.));
#10097=CARTESIAN_POINT('Origin',(-18.,-1.98670067136756E-15,2.));
#10098=CARTESIAN_POINT('Origin',(-18.,-2.,2.));
#10099=CARTESIAN_POINT('Origin',(30.,86.8498045122456,2.));
#10100=CARTESIAN_POINT('Origin',(30.,-13.,25.));
#10101=CARTESIAN_POINT('Origin',(30.,-13.,23.));
#10102=CARTESIAN_POINT('Origin',(-3.28761363381793,-13.,23.));
#10103=CARTESIAN_POINT('Origin',(-18.,-13.,23.));
#10104=CARTESIAN_POINT('Origin',(30.,-13.,23.));
#10105=CARTESIAN_POINT('Origin',(-18.,-13.,23.));
#10106=CARTESIAN_POINT('Origin',(-18.,-13.,23.));
#10107=CARTESIAN_POINT('Origin',(-18.,-2.,2.));
#10108=CARTESIAN_POINT('Origin',(-18.,-2.,2.));
#10109=CARTESIAN_POINT('Origin',(-18.,-2.,2.));
#10110=CARTESIAN_POINT('Origin',(30.,-13.,23.));
#10111=CARTESIAN_POINT('Origin',(30.,-13.,23.));
#10112=CARTESIAN_POINT('Origin',(-18.,19.7279394918662,23.));
#10113=CARTESIAN_POINT('Origin',(-18.,-2.,23.));
#10114=CARTESIAN_POINT('Origin',(-18.,-2.,25.));
#10115=CARTESIAN_POINT('Origin',(-18.,-2.,23.));
#10116=CARTESIAN_POINT('Origin',(2.44929359829471E-16,-2.,2.));
#10117=CARTESIAN_POINT('Origin',(-0.169896300137657,-2.,2.));
#10118=CARTESIAN_POINT('Origin',(55.3717972015101,68.8171894196414,2.));
#10119=CARTESIAN_POINT('Origin',(1.74109754333981,78.4546297413593,2.));
#10120=CARTESIAN_POINT('Origin',(50.,-75.4117474694202,2.));
#10121=CARTESIAN_POINT('Origin',(1.74109754333982,78.4546297413593,2.));
#10122=CARTESIAN_POINT('Origin',(30.,84.6000761633705,25.));
#10123=CARTESIAN_POINT('Origin',(30.,84.6000761633705,23.));
#10124=CARTESIAN_POINT('Origin',(30.,19.7279394918662,23.));
#10125=CARTESIAN_POINT('Origin',(30.,84.6000761633705,23.));
#10126=CARTESIAN_POINT('Origin',(-18.,-2.,23.));
#10127=CARTESIAN_POINT('Origin',(-18.,-2.,23.));
#10128=CARTESIAN_POINT('Origin',(-0.169896300137657,2.,2.));
#10129=CARTESIAN_POINT('Origin',(-0.169896300137657,2.,2.));
#10130=CARTESIAN_POINT('Origin',(1.74109754333981,78.4546297413593,2.));
#10131=CARTESIAN_POINT('Origin',(1.74109754333981,78.4546297413593,2.));
#10132=CARTESIAN_POINT('Origin',(30.,84.6000761633705,23.));
#10133=CARTESIAN_POINT('Origin',(30.,84.6000761633705,23.));
#10134=CARTESIAN_POINT('Origin',(-3.28761363381793,-2.,23.));
#10135=CARTESIAN_POINT('Origin',(-0.169896300137657,-2.,23.));
#10136=CARTESIAN_POINT('Origin',(-0.169896300137657,2.,25.));
#10137=CARTESIAN_POINT('Origin',(-0.169896300137657,2.,23.));
#10138=CARTESIAN_POINT('Origin',(1.74109754333982,78.4546297413593,25.));
#10139=CARTESIAN_POINT('Origin',(1.74109754333982,78.4546297413593,23.));
#10140=CARTESIAN_POINT('Origin',(50.,-75.4117474694202,23.));
#10141=CARTESIAN_POINT('Origin',(1.74109754333981,78.4546297413593,23.));
#10142=CARTESIAN_POINT('Origin',(-0.169896300137657,2.,23.));
#10143=CARTESIAN_POINT('Origin',(1.74109754333981,78.4546297413593,23.));
#10144=CARTESIAN_POINT('Origin',(1.74109754333981,78.4546297413593,23.));
#10145=CARTESIAN_POINT('Origin',(55.3717972015101,68.8171894196414,23.));
#10146=CARTESIAN_POINT('Origin',(-3.58124390253522,-5.29115334922921,5.70951949982205));
#10147=CARTESIAN_POINT('',(-5.15759532720172,-6.25691439705264,9.86573616141742));
#10148=CARTESIAN_POINT('',(-5.15759532720173,-4.03981623667055,1.63018293974891));
#10149=CARTESIAN_POINT('Origin',(-5.06582345881426,-6.27532846007085,9.90101997972383));
#10150=CARTESIAN_POINT('',(0.181310525678022,-7.32816804537255,11.918402053243));
#10151=CARTESIAN_POINT('Origin',(-0.0959656635925021,-4.00763402631843,
-0.315877705231196));
#10152=CARTESIAN_POINT('',(0.0234743673904921,-4.00687461789525,-0.361799188859744));
#10153=CARTESIAN_POINT('Origin',(11.453888025434,17.5975259767542,29.7255459071844));
#10154=CARTESIAN_POINT('Origin',(9.85030394827583,-2.21549538421888,-10.5620593400126));
#10155=CARTESIAN_POINT('',(0.,0.,0.));
#10156=CARTESIAN_POINT('',(0.,0.,0.));
#10157=CARTESIAN_POINT('Origin',(-16.3495307931818,0.,-13.5491970462687));
#10158=CARTESIAN_POINT('',(-15.1213202922933,2.27257763076018,-0.256303827455242));
#10159=CARTESIAN_POINT('',(-15.1213202922933,-2.27257763076018,-0.256303827455243));
#10160=CARTESIAN_POINT('Ctrl Pts',(-15.1213202922914,2.27257763075913,-0.256303827457184));
#10161=CARTESIAN_POINT('Ctrl Pts',(-15.0515142687323,2.23485109064003,-0.326109851015821));
#10162=CARTESIAN_POINT('Ctrl Pts',(-14.9635999263237,2.18198234976026,-0.389326304386628));
#10163=CARTESIAN_POINT('Ctrl Pts',(-14.7279251205928,2.02003601855949,-0.515618311313952));
#10164=CARTESIAN_POINT('Ctrl Pts',(-14.5398271293955,1.85535578506882,-0.550855368407477));
#10165=CARTESIAN_POINT('Ctrl Pts',(-14.2038906955615,1.46968867782391,-0.54663177315069));
#10166=CARTESIAN_POINT('Ctrl Pts',(-14.0399657872398,1.1984002224899,-0.484906409913535));
#10167=CARTESIAN_POINT('Ctrl Pts',(-13.8212117604045,0.614696166914028,
-0.364038582843676));
#10168=CARTESIAN_POINT('Ctrl Pts',(-13.76629442724,0.301085199472153,-0.310906216990201));
#10169=CARTESIAN_POINT('Ctrl Pts',(-13.76629442724,-0.301085199472153,-0.310906216990201));
#10170=CARTESIAN_POINT('Ctrl Pts',(-13.8212117604045,-0.614696166914028,
-0.364038582843676));
#10171=CARTESIAN_POINT('Ctrl Pts',(-14.0399657872398,-1.1984002224899,-0.484906409913535));
#10172=CARTESIAN_POINT('Ctrl Pts',(-14.2038906955615,-1.46968867782391,
-0.54663177315069));
#10173=CARTESIAN_POINT('Ctrl Pts',(-14.5398271293955,-1.85535578506882,
-0.550855368407477));
#10174=CARTESIAN_POINT('Ctrl Pts',(-14.7279251205928,-2.02003601855949,
-0.515618311313952));
#10175=CARTESIAN_POINT('Ctrl Pts',(-14.9635999263244,-2.18198234976076,
-0.389326304386245));
#10176=CARTESIAN_POINT('Ctrl Pts',(-15.0515142687339,-2.23485109064098,
-0.326109851014598));
#10177=CARTESIAN_POINT('Ctrl Pts',(-15.1213202922933,-2.27257763076018,
-0.256303827455241));
#10178=CARTESIAN_POINT('',(-15.69906163763,-2.5,0.321437517881415));
#10179=CARTESIAN_POINT('Origin',(-16.3495307931561,-6.40168473786673E-11,
0.971906673407791));
#10180=CARTESIAN_POINT('',(-15.69906163763,-2.5,-2.248258735165));
#10181=CARTESIAN_POINT('',(-15.69906163763,-2.5,-13.5491970462687));
#10182=CARTESIAN_POINT('',(-16.9999999487337,-2.5,-3.5491970462687));
#10183=CARTESIAN_POINT('Origin',(-16.3495307931821,1.13797860024079E-12,
-2.89872789071702));
#10184=CARTESIAN_POINT('',(-16.9999999487337,-2.5,2.4508029537313));
#10185=CARTESIAN_POINT('',(-16.9999999487337,-2.5,-13.5491970462687));
#10186=CARTESIAN_POINT('',(-16.9999999487337,2.5,2.4508029537313));
#10187=CARTESIAN_POINT('Origin',(-16.3495307931818,-1.27675647831893E-14,
3.10127210928315));
#10188=CARTESIAN_POINT('',(-16.9999999487337,2.5,-3.5491970462687));
#10189=CARTESIAN_POINT('',(-16.9999999487337,2.5,-13.5491970462687));
#10190=CARTESIAN_POINT('',(-15.69906163763,2.5,-2.248258735165));
#10191=CARTESIAN_POINT('Origin',(-16.3495307931817,-2.70228284193763E-12,
-2.89872789071671));
#10192=CARTESIAN_POINT('',(-15.69906163763,2.5,0.321437517881415));
#10193=CARTESIAN_POINT('',(-15.69906163763,2.5,-13.5491970462687));
#10194=CARTESIAN_POINT('Origin',(-16.3495307931675,4.20433132752862E-11,
0.971906673418779));
#10195=CARTESIAN_POINT('Origin',(-0.362549034825799,5.5798767903013,40.6388167522632));
#10196=CARTESIAN_POINT('',(-0.362549034825799,4.4201232096987,42.1388167522632));
#10197=CARTESIAN_POINT('Origin',(-0.362549034825799,4.4201232096987,40.6388167522632));
#10198=CARTESIAN_POINT('',(-0.362549034825799,-4.4201232096987,42.1388167522632));
#10199=CARTESIAN_POINT('',(-0.362549034825799,5.5798767903013,42.1388167522632));
#10200=CARTESIAN_POINT('Origin',(-0.362549034825799,-4.4201232096987,40.6388167522632));
#10201=CARTESIAN_POINT('Origin',(-18.0355338546664,-5.4201232096987,-1.58473095220143));
#10202=CARTESIAN_POINT('',(-18.0355338546664,5.4198767903013,-2.58473095220143));
#10203=CARTESIAN_POINT('Origin',(-18.0355338546664,5.4198767903013,-1.58473095220143));
#10204=CARTESIAN_POINT('',(-18.0355338546664,4.4201232096987,-2.58473095220143));
#10205=CARTESIAN_POINT('',(-18.0355338546664,-5.4201232096987,-2.58473095220143));
#10206=CARTESIAN_POINT('Origin',(-18.0355338546664,4.4201232096987,-1.58473095220143));
#10207=CARTESIAN_POINT('Origin',(-18.0355338546664,-5.4201232096987,-1.58473095220143));
#10208=CARTESIAN_POINT('',(-18.0355338546664,-4.4201232096987,-2.58473095220143));
#10209=CARTESIAN_POINT('Origin',(-18.0355338546664,-4.4201232096987,-1.58473095220143));
#10210=CARTESIAN_POINT('',(-18.0355338546664,-5.4201232096987,-2.58473095220143));
#10211=CARTESIAN_POINT('',(-18.0355338546664,-5.4201232096987,-2.58473095220143));
#10212=CARTESIAN_POINT('Origin',(-18.0355338546664,-5.4201232096987,-1.58473095220143));
#10213=CARTESIAN_POINT('Origin',(-18.0355338546664,-5.4201232096987,-1.58473095220143));
#10214=CARTESIAN_POINT('',(-18.0355338546664,2.5,-2.58473095220143));
#10215=CARTESIAN_POINT('Origin',(-18.0355338546664,2.5,-1.58473095220143));
#10216=CARTESIAN_POINT('',(-18.0355338546664,-2.5,-2.58473095220143));
#10217=CARTESIAN_POINT('',(-18.0355338546664,-5.4201232096987,-2.58473095220143));
#10218=CARTESIAN_POINT('Origin',(-18.0355338546664,-2.5,-1.58473095220143));
#10219=CARTESIAN_POINT('Origin',(0.,18.,8.9205064589513));
#10220=CARTESIAN_POINT('',(-1.83697019872103E-16,-7.5,10.4205064589513));
#10221=CARTESIAN_POINT('Origin',(0.,-7.5,8.9205064589513));
#10222=CARTESIAN_POINT('',(-4.90834909410717E-16,-12.8181093831741,10.4205064589513));
#10223=CARTESIAN_POINT('',(-1.83697019872103E-16,18.,10.4205064589513));
#10224=CARTESIAN_POINT('',(1.27014494349635E-22,-12.8704745779587,7.4205064589513));
#10225=CARTESIAN_POINT('Ctrl Pts',(-6.59194920871187E-16,-12.8181093831741,
10.4205064589513));
#10226=CARTESIAN_POINT('Ctrl Pts',(-0.188255416016175,-12.8181093831741,
10.4205064589513));
#10227=CARTESIAN_POINT('Ctrl Pts',(-0.388988082274336,-12.8141939984886,
10.382902535549));
#10228=CARTESIAN_POINT('Ctrl Pts',(-0.758190528251416,-12.8003284816585,
10.2301098837158));
#10229=CARTESIAN_POINT('Ctrl Pts',(-0.92667197373005,-12.7906121431377,
10.114928217594));
#10230=CARTESIAN_POINT('Ctrl Pts',(-1.19277418140575,-12.7732022326273,
9.8492775803417));
#10231=CARTESIAN_POINT('Ctrl Pts',(-1.30822298061652,-12.7643815870671,
9.68105805060626));
#10232=CARTESIAN_POINT('Ctrl Pts',(-1.46164584377514,-12.7542036356865,
9.31226849459714));
#10233=CARTESIAN_POINT('Ctrl Pts',(-1.49961339720195,-12.7530891067545,
9.1116890996567));
#10234=CARTESIAN_POINT('Ctrl Pts',(-1.50038190415455,-12.7596246829664,
8.73468650392867));
#10235=CARTESIAN_POINT('Ctrl Pts',(-1.46294688463921,-12.7677413612085,
8.53336354542309));
#10236=CARTESIAN_POINT('Ctrl Pts',(-1.31017366956046,-12.7908167965405,
8.16318338701933));
#10237=CARTESIAN_POINT('Ctrl Pts',(-1.19484729740032,-12.8055313315293,
7.9943061245009));
#10238=CARTESIAN_POINT('Ctrl Pts',(-0.928670576176699,-12.8322493038568,
7.72758625806842));
#10239=CARTESIAN_POINT('Ctrl Pts',(-0.760025360862946,-12.8460029733389,
7.61189577191482));
#10240=CARTESIAN_POINT('Ctrl Pts',(-0.390125974594805,-12.8652326714021,
7.45834976030836));
#10241=CARTESIAN_POINT('Ctrl Pts',(-0.188854595603413,-12.8704745779587,
7.4205064589513));
#10242=CARTESIAN_POINT('Ctrl Pts',(-6.93889390390723E-17,-12.8704745779587,
7.4205064589513));
#10243=CARTESIAN_POINT('Ctrl Pts',(3.46944695195361E-17,-12.8704745779587,
7.4205064589513));
#10244=CARTESIAN_POINT('Ctrl Pts',(0.188854595603413,-12.8704745779587,
7.4205064589513));
#10245=CARTESIAN_POINT('Ctrl Pts',(0.390125974594805,-12.8652326714021,
7.45834976030836));
#10246=CARTESIAN_POINT('Ctrl Pts',(0.760025360862947,-12.8460029733389,
7.61189577191482));
#10247=CARTESIAN_POINT('Ctrl Pts',(0.928670576176699,-12.8322493038568,
7.72758625806842));
#10248=CARTESIAN_POINT('Ctrl Pts',(1.19484729740032,-12.8055313315293,7.9943061245009));
#10249=CARTESIAN_POINT('Ctrl Pts',(1.31017366956046,-12.7908167965405,8.16318338701932));
#10250=CARTESIAN_POINT('Ctrl Pts',(1.4629468846392,-12.7677413612085,8.53336354542309));
#10251=CARTESIAN_POINT('Ctrl Pts',(1.50038190415455,-12.7596246829664,8.73468650392867));
#10252=CARTESIAN_POINT('Ctrl Pts',(1.49999688350216,-12.7563503706022,8.92356415151605));
#10253=CARTESIAN_POINT('Ctrl Pts',(1.49961339720195,-12.7530891067545,9.1116890996567));
#10254=CARTESIAN_POINT('Ctrl Pts',(1.46164584377514,-12.7542036356865,9.31226849459714));
#10255=CARTESIAN_POINT('Ctrl Pts',(1.30822298061652,-12.7643815870671,9.68105805060626));
#10256=CARTESIAN_POINT('Ctrl Pts',(1.19277418140575,-12.7732022326273,9.8492775803417));
#10257=CARTESIAN_POINT('Ctrl Pts',(0.92667197373005,-12.7906121431377,10.114928217594));
#10258=CARTESIAN_POINT('Ctrl Pts',(0.758190528251416,-12.8003284816585,
10.2301098837158));
#10259=CARTESIAN_POINT('Ctrl Pts',(0.388988082274337,-12.8141939984886,
10.382902535549));
#10260=CARTESIAN_POINT('Ctrl Pts',(0.188255416016175,-12.8181093831741,
10.4205064589513));
#10261=CARTESIAN_POINT('Ctrl Pts',(-3.46944695195361E-16,-12.8181093831741,
10.4205064589513));
#10262=CARTESIAN_POINT('Origin',(0.,18.,8.9205064589513));
#10263=CARTESIAN_POINT('',(3.48148271110767E-13,12.8704745779592,7.42050645894779));
#10264=CARTESIAN_POINT('',(-5.11233613721112E-18,12.8181093831741,10.4205064589513));
#10265=CARTESIAN_POINT('Ctrl Pts',(-5.20417042793042E-16,12.8704745779587,
7.4205064589513));
#10266=CARTESIAN_POINT('Ctrl Pts',(-0.188854595603414,12.8704745779587,
7.4205064589513));
#10267=CARTESIAN_POINT('Ctrl Pts',(-0.390125974594806,12.8652326714021,
7.45834976030836));
#10268=CARTESIAN_POINT('Ctrl Pts',(-0.760025360862947,12.8460029733389,
7.61189577191482));
#10269=CARTESIAN_POINT('Ctrl Pts',(-0.9286705761767,12.8322493038568,7.72758625806842));
#10270=CARTESIAN_POINT('Ctrl Pts',(-1.19484729740032,12.8055313315293,7.9943061245009));
#10271=CARTESIAN_POINT('Ctrl Pts',(-1.31017366956046,12.7908167965405,8.16318338701933));
#10272=CARTESIAN_POINT('Ctrl Pts',(-1.46294688463921,12.7677413612085,8.53336354542309));
#10273=CARTESIAN_POINT('Ctrl Pts',(-1.50038190415455,12.7596246829664,8.73468650392867));
#10274=CARTESIAN_POINT('Ctrl Pts',(-1.49961339720195,12.7530891067545,9.1116890996567));
#10275=CARTESIAN_POINT('Ctrl Pts',(-1.46164584377514,12.7542036356865,9.31226849459714));
#10276=CARTESIAN_POINT('Ctrl Pts',(-1.30822298061652,12.7643815870671,9.68105805060626));
#10277=CARTESIAN_POINT('Ctrl Pts',(-1.19277418140575,12.7732022326273,9.8492775803417));
#10278=CARTESIAN_POINT('Ctrl Pts',(-0.92667197373005,12.7906121431377,10.114928217594));
#10279=CARTESIAN_POINT('Ctrl Pts',(-0.758190528251416,12.8003284816585,
10.2301098837158));
#10280=CARTESIAN_POINT('Ctrl Pts',(-0.388988082274336,12.8141939984886,
10.382902535549));
#10281=CARTESIAN_POINT('Ctrl Pts',(-0.188255416016174,12.8181093831741,
10.4205064589513));
#10282=CARTESIAN_POINT('Ctrl Pts',(1.73472347597681E-16,12.8181093831741,
10.4205064589513));
#10283=CARTESIAN_POINT('',(-1.83697019872103E-16,7.5,10.4205064589513));
#10284=CARTESIAN_POINT('',(-1.83697019872103E-16,18.,10.4205064589513));
#10285=CARTESIAN_POINT('Origin',(0.,7.5,8.9205064589513));
#10286=CARTESIAN_POINT('Ctrl Pts',(2.42861286636753E-16,12.8181093831741,
10.4205064589513));
#10287=CARTESIAN_POINT('Ctrl Pts',(0.188255416016175,12.8181093831741,10.4205064589513));
#10288=CARTESIAN_POINT('Ctrl Pts',(0.388988082274337,12.8141939984886,10.382902535549));
#10289=CARTESIAN_POINT('Ctrl Pts',(0.758190528251416,12.8003284816585,10.2301098837158));
#10290=CARTESIAN_POINT('Ctrl Pts',(0.92667197373005,12.7906121431377,10.114928217594));
#10291=CARTESIAN_POINT('Ctrl Pts',(1.19277418140575,12.7732022326273,9.8492775803417));
#10292=CARTESIAN_POINT('Ctrl Pts',(1.30822298061652,12.7643815870671,9.68105805060626));
#10293=CARTESIAN_POINT('Ctrl Pts',(1.46164584377514,12.7542036356865,9.31226849459714));
#10294=CARTESIAN_POINT('Ctrl Pts',(1.49961339720195,12.7530891067545,9.1116890996567));
#10295=CARTESIAN_POINT('Ctrl Pts',(1.49999688350216,12.7563503706022,8.92356415151605));
#10296=CARTESIAN_POINT('Ctrl Pts',(1.50038190415455,12.7596246829664,8.73468650392867));
#10297=CARTESIAN_POINT('Ctrl Pts',(1.46294688463921,12.7677413612085,8.53336354542309));
#10298=CARTESIAN_POINT('Ctrl Pts',(1.31017366956046,12.7908167965405,8.16318338701933));
#10299=CARTESIAN_POINT('Ctrl Pts',(1.19484729740032,12.8055313315293,7.9943061245009));
#10300=CARTESIAN_POINT('Ctrl Pts',(0.9286705761767,12.8322493038568,7.72758625806842));
#10301=CARTESIAN_POINT('Ctrl Pts',(0.760025360862947,12.8460029733389,7.61189577191482));
#10302=CARTESIAN_POINT('Ctrl Pts',(0.390125974594805,12.8652326714021,7.45834976030836));
#10303=CARTESIAN_POINT('Ctrl Pts',(0.188854595603413,12.8704745779587,7.4205064589513));
#10304=CARTESIAN_POINT('Ctrl Pts',(-3.12250225675825E-16,12.8704745779587,
7.4205064589513));
#10305=CARTESIAN_POINT('Origin',(0.,0.,0.));
#10306=CARTESIAN_POINT('',(10.3188329323468,7.5,13.9500588701352));
#10307=CARTESIAN_POINT('',(10.3188329323468,-7.5,13.9500588701352));
#10308=CARTESIAN_POINT('Origin',(0.,-3.20084840464449E-15,13.9500588701352));
#10309=CARTESIAN_POINT('',(10.5234605864397,7.5,4.43505886189467));
#10310=CARTESIAN_POINT('Ctrl Pts',(10.5234605864397,7.5,4.43505886189467));
#10311=CARTESIAN_POINT('Ctrl Pts',(10.4554775566161,7.5,7.60673038759669));
#10312=CARTESIAN_POINT('Ctrl Pts',(10.3872728229393,7.5,10.7783971699111));
#10313=CARTESIAN_POINT('Ctrl Pts',(10.3188329323468,7.5,13.9500588701352));
#10314=CARTESIAN_POINT('',(-12.2171188071335,4.42012220175077,0.45080521673159));
#10315=CARTESIAN_POINT('Ctrl Pts',(-12.2171188071335,4.42012220175077,0.45080521673159));
#10316=CARTESIAN_POINT('Ctrl Pts',(-12.149193478595,4.60591899525001,0.488759771825113));
#10317=CARTESIAN_POINT('Ctrl Pts',(-12.0770449733107,4.78999316985353,0.528777321711783));
#10318=CARTESIAN_POINT('Ctrl Pts',(-11.3399329531583,6.55066928002488,0.933845289815028));
#10319=CARTESIAN_POINT('Ctrl Pts',(-10.3575640140156,7.97284514437303,1.44149284263778));
#10320=CARTESIAN_POINT('Ctrl Pts',(-8.09951890179413,10.2431792877324,2.43522522106934));
#10321=CARTESIAN_POINT('Ctrl Pts',(-6.65236232722211,11.2433607265677,2.99343799717399));
#10322=CARTESIAN_POINT('Ctrl Pts',(-3.44419640635119,12.5847950346659,3.93990450984751));
#10323=CARTESIAN_POINT('Ctrl Pts',(-1.68108758943671,12.9245387443403,4.32317244135388));
#10324=CARTESIAN_POINT('Ctrl Pts',(0.803506534154167,12.9184636999382,4.67121150205686));
#10325=CARTESIAN_POINT('Ctrl Pts',(1.63698452641698,12.8407190060581,4.75873226104488));
#10326=CARTESIAN_POINT('Ctrl Pts',(3.29840062387174,12.515315106766,4.87233692567569));
#10327=CARTESIAN_POINT('Ctrl Pts',(4.12633991403241,12.2676894643164,4.89849962173473));
#10328=CARTESIAN_POINT('Ctrl Pts',(6.51022783913382,11.2852931824372,4.89403054082346));
#10329=CARTESIAN_POINT('Ctrl Pts',(7.96408954980376,10.2968570319164,4.77790964454782));
#10330=CARTESIAN_POINT('Ctrl Pts',(9.61578027154998,8.65854700523749,4.57553905407656));
#10331=CARTESIAN_POINT('Ctrl Pts',(10.0927434332412,8.10222543194356,4.50574481122557));
#10332=CARTESIAN_POINT('Ctrl Pts',(10.5234605864397,7.5,4.43505886189466));
#10333=CARTESIAN_POINT('',(-12.1056850526147,4.4201232096987,6.45080295373131));
#10334=CARTESIAN_POINT('Ctrl Pts',(-12.2171206478751,4.4201232096987,0.450804188182521));
#10335=CARTESIAN_POINT('Ctrl Pts',(-12.1982666930902,4.4201232096987,1.46639559259794));
#10336=CARTESIAN_POINT('Ctrl Pts',(-12.1794098522964,4.4201232096987,2.48198817833168));
#10337=CARTESIAN_POINT('Ctrl Pts',(-12.1605478920539,4.4201232096987,3.49758066897254));
#10338=CARTESIAN_POINT('Ctrl Pts',(-12.1422651106841,4.4201232096987,4.48198818698683));
#10339=CARTESIAN_POINT('Ctrl Pts',(-12.1239775194361,4.4201232096987,5.46639561565845));
#10340=CARTESIAN_POINT('Ctrl Pts',(-12.1056850526147,4.4201232096987,6.45080295373131));
#10341=CARTESIAN_POINT('',(-12.8874008156035,1.57825141581578E-15,6.45080295373131));
#10342=CARTESIAN_POINT('Origin',(0.,0.,6.45080295373131));
#10343=CARTESIAN_POINT('',(-12.4283466236009,9.69183562681548E-16,32.75));
#10344=CARTESIAN_POINT('',(-13.,1.59204083889156E-15,0.));
#10345=CARTESIAN_POINT('',(12.4283599700267,-2.15362009418406E-15,32.7492353837737));
#10346=CARTESIAN_POINT('Ctrl Pts',(-12.4283466236009,6.93889390390723E-16,
32.75));
#10347=CARTESIAN_POINT('Ctrl Pts',(-12.4283466236009,0.794308918128955,
32.75));
#10348=CARTESIAN_POINT('Ctrl Pts',(-12.3502527632816,1.61021372884421,32.7930538414047));
#10349=CARTESIAN_POINT('Ctrl Pts',(-12.0274177529636,3.22310913323241,32.9643815831464));
#10350=CARTESIAN_POINT('Ctrl Pts',(-11.7828051502509,4.0201542931032,33.0923838793489));
#10351=CARTESIAN_POINT('Ctrl Pts',(-10.8223388252417,6.3016876936436,33.5641120509972));
#10352=CARTESIAN_POINT('Ctrl Pts',(-9.86802331505246,7.67569650721005,33.9952885548655));
#10353=CARTESIAN_POINT('Ctrl Pts',(-7.68673433352581,9.84141368018456,34.7773406223861));
#10354=CARTESIAN_POINT('Ctrl Pts',(-6.30675051410171,10.7871492962387,35.1838249513449));
#10355=CARTESIAN_POINT('Ctrl Pts',(-4.01853645200771,11.7370350358201,35.6118527441021));
#10356=CARTESIAN_POINT('Ctrl Pts',(-3.21987048035003,11.9784899796951,35.7251137378412));
#10357=CARTESIAN_POINT('Ctrl Pts',(-1.60639827951172,12.2965977499602,35.8754701561768));
#10358=CARTESIAN_POINT('Ctrl Pts',(-0.791562918351071,12.3731454095824,
35.9124754330905));
#10359=CARTESIAN_POINT('Ctrl Pts',(0.791571803892222,12.3731461491244,35.9124330647567));
#10360=CARTESIAN_POINT('Ctrl Pts',(1.60641400117091,12.296597562387,35.875383360731));
#10361=CARTESIAN_POINT('Ctrl Pts',(3.21989600364048,11.9784866527797,35.7249372434734));
#10362=CARTESIAN_POINT('Ctrl Pts',(4.01856495072364,11.7370295233017,35.6116309738994));
#10363=CARTESIAN_POINT('Ctrl Pts',(6.30678393558675,10.7871375666671,35.1834705050684));
#10364=CARTESIAN_POINT('Ctrl Pts',(7.68676566759693,9.84139890551597,34.7769017525103));
#10365=CARTESIAN_POINT('Ctrl Pts',(9.8680427591823,7.67568550857489,33.9947109969587));
#10366=CARTESIAN_POINT('Ctrl Pts',(10.8223529970034,6.30168425346591,33.5634693670658));
#10367=CARTESIAN_POINT('Ctrl Pts',(11.7828170674242,4.02015736730738,33.0916705623065));
#10368=CARTESIAN_POINT('Ctrl Pts',(12.0274298028565,3.22311347643651,32.9636492417211));
#10369=CARTESIAN_POINT('Ctrl Pts',(12.3502655341755,1.61021795970926,32.7922958208113));
#10370=CARTESIAN_POINT('Ctrl Pts',(12.4283599700267,0.794311754446631,32.7492353837737));
#10371=CARTESIAN_POINT('Ctrl Pts',(12.4283599700267,1.38777878078145E-16,
32.7492353837737));
#10372=CARTESIAN_POINT('Ctrl Pts',(12.4283599700267,-2.77555756156289E-16,
32.7492353837737));
#10373=CARTESIAN_POINT('Ctrl Pts',(12.4283599700267,-0.794311754446632,
32.7492353837737));
#10374=CARTESIAN_POINT('Ctrl Pts',(12.3502655341755,-1.61021795970926,32.7922958208113));
#10375=CARTESIAN_POINT('Ctrl Pts',(12.0274298028565,-3.22311347643651,32.9636492417211));
#10376=CARTESIAN_POINT('Ctrl Pts',(11.7828170674242,-4.02015736730738,33.0916705623065));
#10377=CARTESIAN_POINT('Ctrl Pts',(10.8223529970034,-6.30168425346592,33.5634693670658));
#10378=CARTESIAN_POINT('Ctrl Pts',(9.8680427591823,-7.6756855085749,33.9947109969587));
#10379=CARTESIAN_POINT('Ctrl Pts',(7.68676566759692,-9.84139890551598,34.7769017525103));
#10380=CARTESIAN_POINT('Ctrl Pts',(6.30678393558675,-10.7871375666671,35.1834705050684));
#10381=CARTESIAN_POINT('Ctrl Pts',(4.01856495072364,-11.7370295233017,35.6116309738994));
#10382=CARTESIAN_POINT('Ctrl Pts',(3.21989600364047,-11.9784866527797,35.7249372434734));
#10383=CARTESIAN_POINT('Ctrl Pts',(1.60641400117091,-12.296597562387,35.875383360731));
#10384=CARTESIAN_POINT('Ctrl Pts',(0.791571803892224,-12.3731461491244,
35.9124330647567));
#10385=CARTESIAN_POINT('Ctrl Pts',(-0.791562918351067,-12.3731454095824,
35.9124754330905));
#10386=CARTESIAN_POINT('Ctrl Pts',(-1.60639827951171,-12.2965977499602,
35.8754701561768));
#10387=CARTESIAN_POINT('Ctrl Pts',(-3.21987048035002,-11.9784899796951,
35.7251137378412));
#10388=CARTESIAN_POINT('Ctrl Pts',(-4.0185364520077,-11.7370350358201,35.6118527441021));
#10389=CARTESIAN_POINT('Ctrl Pts',(-6.30675051410171,-10.7871492962387,
35.1838249513449));
#10390=CARTESIAN_POINT('Ctrl Pts',(-7.68673433352581,-9.84141368018457,
34.7773406223861));
#10391=CARTESIAN_POINT('Ctrl Pts',(-9.86802331505246,-7.67569650721005,
33.9952885548655));
#10392=CARTESIAN_POINT('Ctrl Pts',(-10.8223388252417,-6.3016876936436,33.5641120509972));
#10393=CARTESIAN_POINT('Ctrl Pts',(-11.7828051502509,-4.0201542931032,33.0923838793489));
#10394=CARTESIAN_POINT('Ctrl Pts',(-12.0274177529636,-3.22310913323241,
32.9643815831464));
#10395=CARTESIAN_POINT('Ctrl Pts',(-12.3502527632816,-1.61021372884421,
32.7930538414047));
#10396=CARTESIAN_POINT('Ctrl Pts',(-12.4283466236009,-0.794308918128954,
32.75));
#10397=CARTESIAN_POINT('Ctrl Pts',(-12.4283466236009,0.,32.75));
#10398=CARTESIAN_POINT('',(-12.1056850526147,-4.4201232096987,6.45080295373131));
#10399=CARTESIAN_POINT('Origin',(0.,0.,6.45080295373131));
#10400=CARTESIAN_POINT('',(-12.2171192862399,-4.4201226050411,0.450804099959431));
#10401=CARTESIAN_POINT('Ctrl Pts',(-12.1056850526147,-4.4201232096987,6.45080295373131));
#10402=CARTESIAN_POINT('Ctrl Pts',(-12.1239775194361,-4.4201232096987,5.46639561565844));
#10403=CARTESIAN_POINT('Ctrl Pts',(-12.1422651106866,-4.4201232096987,4.48198818697493));
#10404=CARTESIAN_POINT('Ctrl Pts',(-12.1605478920564,-4.4201232096987,3.49758066896046));
#10405=CARTESIAN_POINT('Ctrl Pts',(-12.179409852299,-4.4201232096987,2.48198817831942));
#10406=CARTESIAN_POINT('Ctrl Pts',(-12.1982666930902,-4.4201232096987,1.46639559259794));
#10407=CARTESIAN_POINT('Ctrl Pts',(-12.2171206478751,-4.4201232096987,0.45080418818252));
#10408=CARTESIAN_POINT('',(10.5234605864397,-7.5,4.43505886189467));
#10409=CARTESIAN_POINT('Ctrl Pts',(10.5234605864397,-7.50000000000001,4.43505886189466));
#10410=CARTESIAN_POINT('Ctrl Pts',(10.0927434332412,-8.10222543194357,4.50574481122557));
#10411=CARTESIAN_POINT('Ctrl Pts',(9.61578027154998,-8.6585470052375,4.57553905407656));
#10412=CARTESIAN_POINT('Ctrl Pts',(7.96408954980375,-10.2968570319164,4.77790964454782));
#10413=CARTESIAN_POINT('Ctrl Pts',(6.51022783913381,-11.2852931824372,4.89403054082346));
#10414=CARTESIAN_POINT('Ctrl Pts',(4.1263399140324,-12.2676894643164,4.89849962173473));
#10415=CARTESIAN_POINT('Ctrl Pts',(3.29840062387173,-12.515315106766,4.87233692567569));
#10416=CARTESIAN_POINT('Ctrl Pts',(1.63698452641698,-12.8407190060581,4.75873226104488));
#10417=CARTESIAN_POINT('Ctrl Pts',(0.803506534154166,-12.9184636999382,
4.67121150205686));
#10418=CARTESIAN_POINT('Ctrl Pts',(-1.68108758943671,-12.9245387443403,
4.32317244135388));
#10419=CARTESIAN_POINT('Ctrl Pts',(-3.44419640635119,-12.5847950346659,
3.93990450984751));
#10420=CARTESIAN_POINT('Ctrl Pts',(-6.6523623272221,-11.2433607265677,2.99343799717399));
#10421=CARTESIAN_POINT('Ctrl Pts',(-8.09951890179412,-10.2431792877324,
2.43522522106934));
#10422=CARTESIAN_POINT('Ctrl Pts',(-10.3575640140156,-7.97284514437303,
1.44149284263779));
#10423=CARTESIAN_POINT('Ctrl Pts',(-11.3399329531583,-6.55066928002488,
0.933845289815027));
#10424=CARTESIAN_POINT('Ctrl Pts',(-12.0770449733107,-4.78999316985353,
0.528777321711782));
#10425=CARTESIAN_POINT('Ctrl Pts',(-12.149193478595,-4.60591899525002,0.488759771825114));
#10426=CARTESIAN_POINT('Ctrl Pts',(-12.2171188071335,-4.42012220175077,
0.450805216731591));
#10427=CARTESIAN_POINT('Ctrl Pts',(10.3188329323468,-7.5,13.9500588701352));
#10428=CARTESIAN_POINT('Ctrl Pts',(10.3872728229393,-7.5,10.7783971699111));
#10429=CARTESIAN_POINT('Ctrl Pts',(10.4554775566161,-7.5,7.60673038759669));
#10430=CARTESIAN_POINT('Ctrl Pts',(10.5234605864397,-7.5,4.43505886189467));
#10431=CARTESIAN_POINT('Origin',(-12.4644660428009,2.5,-2.91315807694762));
#10432=CARTESIAN_POINT('',(-15.1213202922933,-2.5,-0.256303827455243));
#10433=CARTESIAN_POINT('',(-12.4644660428009,-2.5,-2.91315807694762));
#10434=CARTESIAN_POINT('',(-15.1213202922933,2.5,-0.256303827455242));
#10435=CARTESIAN_POINT('Origin',(-19.5355338546664,-2.5,-9.9842258888131));
#10436=CARTESIAN_POINT('',(-13.7071067299202,-2.5,-0.256303827455243));
#10437=CARTESIAN_POINT('',(-17.9497474170395,-2.5,-4.49894451457453));
#10438=CARTESIAN_POINT('Origin',(-14.4142135111068,-2.5,0.450802953731305));
#10439=CARTESIAN_POINT('Origin',(-19.5355338546664,2.5,-9.9842258888131));
#10440=CARTESIAN_POINT('',(-15.1213202922933,2.5,-0.256303827455243));
#10441=CARTESIAN_POINT('',(-12.4644660428009,2.5,-2.91315807694762));
#10442=CARTESIAN_POINT('',(-13.7071067299202,2.5,-0.256303827455243));
#10443=CARTESIAN_POINT('',(-17.9497474170395,2.5,-4.49894451457453));
#10444=CARTESIAN_POINT('Origin',(-14.4142135111068,2.5,0.450802953731305));
#10445=CARTESIAN_POINT('Origin',(-11.224345965807,0.,-11.224345965807));
#10446=CARTESIAN_POINT('',(-18.656854198226,-4.4201232096987,-3.79183773338798));
#10447=CARTESIAN_POINT('',(-20.242640635853,-4.4201232096987,-2.20605129576108));
#10448=CARTESIAN_POINT('',(-17.9497474170395,-4.4201232096987,-4.49894451457453));
#10449=CARTESIAN_POINT('',(-20.242640635853,-2.5,-2.20605129576108));
#10450=CARTESIAN_POINT('',(-20.242640635853,-2.5,-2.20605129576108));
#10451=CARTESIAN_POINT('',(-18.656854198226,-2.5,-3.79183773338798));
#10452=CARTESIAN_POINT('',(-11.224345965807,-2.5,-11.224345965807));
#10453=CARTESIAN_POINT('',(-18.656854198226,-4.4201232096987,-3.79183773338798));
#10454=CARTESIAN_POINT('Origin',(0.,0.,0.));
#10455=CARTESIAN_POINT('Origin',(0.,0.,0.450802953731306));
#10456=CARTESIAN_POINT('Ctrl Pts',(-12.2171188071335,-4.42012220175077,
0.450805216731591));
#10457=CARTESIAN_POINT('Ctrl Pts',(-12.4437244891765,-3.80028553672204,
0.324185029112939));
#10458=CARTESIAN_POINT('Ctrl Pts',(-12.6230045022273,-3.16110024476212,
0.220809942356288));
#10459=CARTESIAN_POINT('Ctrl Pts',(-12.9188641006425,-1.67701333832259,
0.0485983978862804));
#10460=CARTESIAN_POINT('Ctrl Pts',(-13.,-0.827603999929081,-8.71233909165408E-15));
#10461=CARTESIAN_POINT('Ctrl Pts',(-13.,0.827603999929072,-9.05122930234842E-15));
#10462=CARTESIAN_POINT('Ctrl Pts',(-12.9188641006425,1.67701333832258,0.0485983978862817));
#10463=CARTESIAN_POINT('Ctrl Pts',(-12.6230045022273,3.16110024476212,0.22080994235629));
#10464=CARTESIAN_POINT('Ctrl Pts',(-12.4437244891765,3.80028553672204,0.324185029112938));
#10465=CARTESIAN_POINT('Ctrl Pts',(-12.2171188071335,4.42012220175077,0.45080521673159));
#10466=CARTESIAN_POINT('Origin',(4.85535470457189,36.,-30.1029285680633));
#10467=CARTESIAN_POINT('',(-8.,-7.5,2.45071724035024));
#10468=CARTESIAN_POINT('',(-8.,7.5,2.45071724035023));
#10469=CARTESIAN_POINT('',(-8.,36.,2.45071724035024));
#10470=CARTESIAN_POINT('Origin',(4.85535470457189,-7.5,-30.1029285680633));
#10471=CARTESIAN_POINT('Origin',(4.85535470457189,7.5,-30.1029285680633));
#10472=CARTESIAN_POINT('Origin',(-0.000695819921353427,36.,9.91245425835333));
#10473=CARTESIAN_POINT('',(7.44355606790684,-4.4201232096987,34.8239599099708));
#10474=CARTESIAN_POINT('',(7.44355606790684,4.4201232096987,34.8239599099708));
#10475=CARTESIAN_POINT('',(7.44355606790684,36.,34.8239599099708));
#10476=CARTESIAN_POINT('',(-7.44355606790684,-4.4201232096987,34.8243757283837));
#10477=CARTESIAN_POINT('Origin',(-0.000695819921353427,-4.4201232096987,
9.91245425835333));
#10478=CARTESIAN_POINT('',(-7.44355606790684,4.4201232096987,34.8243757283837));
#10479=CARTESIAN_POINT('',(-7.44355606790684,36.,34.8243757283837));
#10480=CARTESIAN_POINT('Origin',(-0.000695819921353427,4.4201232096987,
9.91245425835333));
#10481=CARTESIAN_POINT('Origin',(16.,7.5,13.9500588701352));
#10482=CARTESIAN_POINT('',(-8.,-7.5,13.9500588701352));
#10483=CARTESIAN_POINT('',(16.,-7.5,13.9500588701352));
#10484=CARTESIAN_POINT('',(-8.,7.5,13.9500588701352));
#10485=CARTESIAN_POINT('',(-8.,7.5,13.9500588701352));
#10486=CARTESIAN_POINT('',(16.,7.5,13.9500588701352));
#10487=CARTESIAN_POINT('Origin',(16.,-7.5,-13.9500588701352));
#10488=CARTESIAN_POINT('',(-8.,-7.5,-13.9500588701352));
#10489=CARTESIAN_POINT('Origin',(16.,7.5,-13.9500588701352));
#10490=CARTESIAN_POINT('',(-8.,7.5,-13.9500588701352));
#10491=CARTESIAN_POINT('Origin',(-8.,0.,0.));
#10492=CARTESIAN_POINT('Origin',(13.2559086557882,-4.4201232096987,0.450802953731306));
#10493=CARTESIAN_POINT('',(-12.9999999487337,-4.4201232096987,0.450802953731307));
#10494=CARTESIAN_POINT('',(13.2559086557882,-4.4201232096987,0.450802953731306));
#10495=CARTESIAN_POINT('',(-12.9999999487337,4.4201232096987,0.450802953731308));
#10496=CARTESIAN_POINT('',(-12.9999999487337,-4.4201232096987,0.450802953731306));
#10497=CARTESIAN_POINT('',(13.2559086557882,4.4201232096987,0.450802953731306));
#10498=CARTESIAN_POINT('Origin',(13.2559086557882,4.4201232096987,6.45080295373131));
#10499=CARTESIAN_POINT('',(-20.242640635853,4.4201232096987,-2.20605129576108));
#10500=CARTESIAN_POINT('',(-18.656854198226,4.4201232096987,-3.79183773338798));
#10501=CARTESIAN_POINT('',(-20.9497474170395,4.4201232096987,-1.49894451457453));
#10502=CARTESIAN_POINT('',(-20.242640635853,4.4201232096987,-0.79183773338798));
#10503=CARTESIAN_POINT('Origin',(-19.5355338546664,4.4201232096987,-1.49894451457453));
#10504=CARTESIAN_POINT('',(-12.9999999487337,4.4201232096987,6.45080295373131));
#10505=CARTESIAN_POINT('',(-20.9497474170395,4.4201232096987,-1.49894451457453));
#10506=CARTESIAN_POINT('',(13.2559086557882,4.4201232096987,6.45080295373131));
#10507=CARTESIAN_POINT('',(-17.2426406358529,4.4201232096987,-3.79183773338798));
#10508=CARTESIAN_POINT('',(-17.9497474170395,4.4201232096987,-4.49894451457453));
#10509=CARTESIAN_POINT('Origin',(-17.9497474170395,4.4201232096987,-3.08473095220143));
#10510=CARTESIAN_POINT('Origin',(13.2559086557882,-4.4201232096987,6.45080295373131));
#10511=CARTESIAN_POINT('',(-12.9999999487337,-4.4201232096987,6.45080295373131));
#10512=CARTESIAN_POINT('',(-12.9999999487337,-4.4201232096987,6.45080295373131));
#10513=CARTESIAN_POINT('',(13.2559086557882,-4.4201232096987,6.45080295373131));
#10514=CARTESIAN_POINT('Origin',(13.2559086557882,-4.4201232096987,6.45080295373131));
#10515=CARTESIAN_POINT('',(-20.242640635853,-4.4201232096987,-0.79183773338798));
#10516=CARTESIAN_POINT('',(-20.9497474170395,-4.4201232096987,-1.49894451457453));
#10517=CARTESIAN_POINT('Origin',(-19.5355338546664,-4.4201232096987,-1.49894451457453));
#10518=CARTESIAN_POINT('',(-17.2426406358529,-4.4201232096987,-3.79183773338798));
#10519=CARTESIAN_POINT('Origin',(-17.9497474170395,-4.4201232096987,-3.08473095220143));
#10520=CARTESIAN_POINT('',(-17.9497474170395,-4.4201232096987,-4.49894451457453));
#10521=CARTESIAN_POINT('Origin',(-17.9497474170395,4.4201232096987,-4.49894451457453));
#10522=CARTESIAN_POINT('',(-17.2426406358529,2.5,-3.79183773338798));
#10523=CARTESIAN_POINT('',(-17.9497474170395,2.5,-4.49894451457453));
#10524=CARTESIAN_POINT('',(-17.2426406358529,4.4201232096987,-3.79183773338798));
#10525=CARTESIAN_POINT('',(-17.2426406358529,-2.5,-3.79183773338798));
#10526=CARTESIAN_POINT('',(-17.2426406358529,-2.5,-3.79183773338798));
#10527=CARTESIAN_POINT('',(-17.9497474170395,-2.5,-4.49894451457453));
#10528=CARTESIAN_POINT('',(-13.7071067299202,4.4201232096987,-0.256303827455243));
#10529=CARTESIAN_POINT('Origin',(-20.9497474170395,-4.4201232096987,-1.49894451457453));
#10530=CARTESIAN_POINT('',(-20.242640635853,2.5,-0.791837733387981));
#10531=CARTESIAN_POINT('',(-24.4852813229722,2.5,-5.03447842050726));
#10532=CARTESIAN_POINT('',(-20.242640635853,-2.5,-0.791837733387981));
#10533=CARTESIAN_POINT('',(-24.4852813229722,-2.5,-5.03447842050726));
#10534=CARTESIAN_POINT('',(-20.242640635853,-4.4201232096987,-0.79183773338798));
#10535=CARTESIAN_POINT('',(-20.242640635853,2.5,-0.79183773338798));
#10536=CARTESIAN_POINT('Origin',(-11.224345965807,0.,-11.224345965807));
#10537=CARTESIAN_POINT('',(-20.242640635853,2.5,-2.20605129576108));
#10538=CARTESIAN_POINT('',(-18.656854198226,2.5,-3.79183773338798));
#10539=CARTESIAN_POINT('',(-11.224345965807,2.5,-11.224345965807));
#10540=CARTESIAN_POINT('',(-20.242640635853,4.4201232096987,-2.20605129576108));
#10541=CARTESIAN_POINT('',(-18.656854198226,2.5,-3.79183773338798));
#10542=CARTESIAN_POINT('Origin',(-12.4644660428009,2.5,-2.91315807694762));
#10543=CARTESIAN_POINT('',(-15.1213202922933,2.5,-0.256303827455242));
#10544=CARTESIAN_POINT('Origin',(-19.5355338546664,-2.5,-9.9842258888131));
#10545=CARTESIAN_POINT('Origin',(-17.9497474170395,-2.5,-3.08473095220143));
#10546=CARTESIAN_POINT('Origin',(-19.5355338546664,-2.5,-1.49894451457453));
#10547=CARTESIAN_POINT('Origin',(-19.5355338546664,2.5,-9.9842258888131));
#10548=CARTESIAN_POINT('Origin',(-19.5355338546664,2.5,-1.49894451457453));
#10549=CARTESIAN_POINT('Origin',(-17.9497474170395,2.5,-3.08473095220143));
#10550=CARTESIAN_POINT('Origin',(-18.0355338546664,-5.4201232096987,-1.58473095220143));
#10551=CARTESIAN_POINT('Origin',(-18.0355338546664,5.4198767903013,-1.58473095220143));
#10552=CARTESIAN_POINT('Origin',(-19.5355338546664,0.,-1.49894451457453));
#10553=CARTESIAN_POINT('Origin',(-19.5355338546664,0.,-1.49894451457453));
#10554=CARTESIAN_POINT('Origin',(-17.9497474170395,0.,-3.08473095220143));
#10555=CARTESIAN_POINT('Origin',(-17.9497474170395,0.,-3.08473095220143));
#10556=CARTESIAN_POINT('Origin',(-14.4142135111068,4.4201232096987,0.450802953731305));
#10557=CARTESIAN_POINT('Origin',(0.,0.,45.));
#10558=CARTESIAN_POINT('',(-4.44355606790684,-4.4201232096987,45.));
#10559=CARTESIAN_POINT('',(4.44355606790684,-4.4201232096987,45.));
#10560=CARTESIAN_POINT('',(7.44355606790684,-4.4201232096987,45.));
#10561=CARTESIAN_POINT('',(4.44355606790684,4.4201232096987,45.));
#10562=CARTESIAN_POINT('',(4.44355606790684,4.4201232096987,45.));
#10563=CARTESIAN_POINT('',(-4.44355606790684,4.4201232096987,45.));
#10564=CARTESIAN_POINT('',(7.44355606790684,4.4201232096987,45.));
#10565=CARTESIAN_POINT('',(-4.44355606790684,-4.4201232096987,45.));
#10566=CARTESIAN_POINT('Origin',(7.44355606790684,-4.4201232096987,-4.08573095220143));
#10567=CARTESIAN_POINT('',(7.44355606790684,-4.4201232096987,42.));
#10568=CARTESIAN_POINT('',(7.44355606790684,-4.4201232096987,-4.08573095220143));
#10569=CARTESIAN_POINT('Origin',(4.44355606790684,-4.4201232096987,42.));
#10570=CARTESIAN_POINT('',(-7.44355606790684,-4.4201232096987,42.));
#10571=CARTESIAN_POINT('Origin',(-4.44355606790684,-4.4201232096987,42.));
#10572=CARTESIAN_POINT('',(-7.44355606790684,-4.4201232096987,-4.08573095220143));
#10573=CARTESIAN_POINT('Origin',(7.44355606790684,4.4201232096987,-4.08573095220143));
#10574=CARTESIAN_POINT('',(7.44355606790684,4.4201232096987,42.));
#10575=CARTESIAN_POINT('',(7.44355606790684,4.4201232096987,-4.08573095220143));
#10576=CARTESIAN_POINT('',(7.44355606790684,-4.4201232096987,42.));
#10577=CARTESIAN_POINT('Origin',(7.44355606790684,4.4201232096987,-4.08573095220143));
#10578=CARTESIAN_POINT('Origin',(4.44355606790684,4.4201232096987,42.));
#10579=CARTESIAN_POINT('',(-7.44355606790684,4.4201232096987,42.));
#10580=CARTESIAN_POINT('',(-7.44355606790684,4.4201232096987,-4.08573095220143));
#10581=CARTESIAN_POINT('Origin',(-4.44355606790684,4.4201232096987,42.));
#10582=CARTESIAN_POINT('Origin',(-7.44355606790684,4.4201232096987,-4.08573095220143));
#10583=CARTESIAN_POINT('',(-7.44355606790684,4.4201232096987,42.));
#10584=CARTESIAN_POINT('Origin',(4.44355606790684,0.,42.));
#10585=CARTESIAN_POINT('Origin',(-4.44355606790684,0.,42.));
#10586=CARTESIAN_POINT('',(0.,0.,0.));
#10587=CARTESIAN_POINT('Origin',(-0.414990954321311,5.02189031698537,38.8542865365866));
#10588=CARTESIAN_POINT('',(-0.414990954321311,3.97811209444304,40.2042865365866));
#10589=CARTESIAN_POINT('Origin',(-0.414990954321311,3.97811209444304,38.8542865365866));
#10590=CARTESIAN_POINT('',(-0.414990954321311,-3.97810968301463,40.2042865365866));
#10591=CARTESIAN_POINT('',(-0.414990954321311,5.02189031698537,40.2042865365866));
#10592=CARTESIAN_POINT('Origin',(-0.414990954321311,-3.97810968301463,38.8542865365866));
#10593=CARTESIAN_POINT('Origin',(-16.3206772921779,-4.87810968301463,0.853093602568413));
#10594=CARTESIAN_POINT('',(-16.3206772921779,4.87789031698537,-0.0469063974315885));
#10595=CARTESIAN_POINT('Origin',(-16.3206772921779,4.87789031698537,0.853093602568413));
#10596=CARTESIAN_POINT('',(-16.3206772921779,3.97811209444304,-0.0469063974315885));
#10597=CARTESIAN_POINT('',(-16.3206772921779,-4.87810968301463,-0.0469063974315885));
#10598=CARTESIAN_POINT('Origin',(-16.3206772921779,3.97811209444304,0.853093602568413));
#10599=CARTESIAN_POINT('Origin',(-16.3206772921779,-4.87810968301463,0.853093602568413));
#10600=CARTESIAN_POINT('',(-16.3206772921779,-3.97810968301463,-0.0469063974315885));
#10601=CARTESIAN_POINT('Origin',(-16.3206772921779,-3.97810968301463,0.853093602568413));
#10602=CARTESIAN_POINT('',(-16.3206772921779,-4.87810968301463,-0.0469063974315885));
#10603=CARTESIAN_POINT('',(-16.3206772921779,-4.87810968301463,-0.0469063974315885));
#10604=CARTESIAN_POINT('Origin',(-16.3206772921779,-4.87810968301463,0.853093602568413));
#10605=CARTESIAN_POINT('Origin',(-16.3206772921779,-4.87810968301463,0.853093602568413));
#10606=CARTESIAN_POINT('',(-16.3206772921779,2.2500012057142,-0.0469063974315885));
#10607=CARTESIAN_POINT('Origin',(-16.3206772921779,2.2500012057142,0.853093602568413));
#10608=CARTESIAN_POINT('',(-16.3206772921779,-2.2499987942858,-0.0469063974315885));
#10609=CARTESIAN_POINT('',(-16.3206772921779,-4.87810968301463,-0.0469063974315885));
#10610=CARTESIAN_POINT('Origin',(-16.3206772921779,-2.2499987942858,0.853093602568413));
#10611=CARTESIAN_POINT('Origin',(-0.0886968229780924,16.2000012057142,10.3078072726059));
#10612=CARTESIAN_POINT('',(-0.0886968229780925,-6.74999879428579,11.6578072726059));
#10613=CARTESIAN_POINT('Origin',(-0.0886968229780924,-6.7499987942858,10.3078072726059));
#10614=CARTESIAN_POINT('',(-0.0886968229780923,-11.5362972391425,11.6578072726059));
#10615=CARTESIAN_POINT('',(-0.0886968229780925,16.2000012057142,11.6578072726059));
#10616=CARTESIAN_POINT('',(-0.0886968229780924,-11.5834259144487,8.95780727260587));
#10617=CARTESIAN_POINT('Ctrl Pts',(-0.0886968229780924,-11.5362972391425,
11.6578072726059));
#10618=CARTESIAN_POINT('Ctrl Pts',(-0.25812669739265,-11.5362972391425,
11.6578072726059));
#10619=CARTESIAN_POINT('Ctrl Pts',(-0.438786097024996,-11.5327733929255,
11.6239637415438));
#10620=CARTESIAN_POINT('Ctrl Pts',(-0.771068298404367,-11.5202944277784,
11.4864503548939));
#10621=CARTESIAN_POINT('Ctrl Pts',(-0.922701599335139,-11.5115497231097,
11.3827868553843));
#10622=CARTESIAN_POINT('Ctrl Pts',(-1.16219358624327,-11.4958808036504,
11.1437012818572));
#10623=CARTESIAN_POINT('Ctrl Pts',(-1.26609750553296,-11.4879422226462,
10.9923037050953));
#10624=CARTESIAN_POINT('Ctrl Pts',(-1.40417808237572,-11.4787820664037,
10.6603931046871));
#10625=CARTESIAN_POINT('Ctrl Pts',(-1.43834888045985,-11.4777789903649,
10.4798716492407));
#10626=CARTESIAN_POINT('Ctrl Pts',(-1.43904053671719,-11.4836610089555,
10.1405693130855));
#10627=CARTESIAN_POINT('Ctrl Pts',(-1.40534901915338,-11.4909660193735,
9.95937865043048));
#10628=CARTESIAN_POINT('Ctrl Pts',(-1.26785312558251,-11.5117339111722,
9.6262165078671));
#10629=CARTESIAN_POINT('Ctrl Pts',(-1.16405939063838,-11.5249769926622,
9.47422697160051));
#10630=CARTESIAN_POINT('Ctrl Pts',(-0.924500341537122,-11.549023167757,
9.23417909181128));
#10631=CARTESIAN_POINT('Ctrl Pts',(-0.772719647754745,-11.5614014702908,
9.13005765427303));
#10632=CARTESIAN_POINT('Ctrl Pts',(-0.439810200113418,-11.5787081985477,
8.99186624382722));
#10633=CARTESIAN_POINT('Ctrl Pts',(-0.258665959021164,-11.5834259144487,
8.95780727260587));
#10634=CARTESIAN_POINT('Ctrl Pts',(-0.0886968229780923,-11.5834259144487,
8.95780727260587));
#10635=CARTESIAN_POINT('Ctrl Pts',(-0.0886968229780924,-11.5834259144487,
8.95780727260587));
#10636=CARTESIAN_POINT('Ctrl Pts',(0.0812723130649798,-11.5834259144487,
8.95780727260587));
#10637=CARTESIAN_POINT('Ctrl Pts',(0.262416554157233,-11.5787081985477,
8.99186624382722));
#10638=CARTESIAN_POINT('Ctrl Pts',(0.595326001798561,-11.5614014702908,
9.13005765427303));
#10639=CARTESIAN_POINT('Ctrl Pts',(0.747106695580938,-11.549023167757,9.23417909181128));
#10640=CARTESIAN_POINT('Ctrl Pts',(0.986665744682193,-11.5249769926622,
9.47422697160051));
#10641=CARTESIAN_POINT('Ctrl Pts',(1.09045947962633,-11.5117339111722,9.6262165078671));
#10642=CARTESIAN_POINT('Ctrl Pts',(1.22795537319719,-11.4909660193735,9.95937865043048));
#10643=CARTESIAN_POINT('Ctrl Pts',(1.261646890761,-11.4836610089555,10.1405693130855));
#10644=CARTESIAN_POINT('Ctrl Pts',(1.26130037217385,-11.4807141278278,10.3105591959141));
#10645=CARTESIAN_POINT('Ctrl Pts',(1.26095523450366,-11.4777789903649,10.4798716492407));
#10646=CARTESIAN_POINT('Ctrl Pts',(1.22678443641954,-11.4787820664037,10.6603931046871));
#10647=CARTESIAN_POINT('Ctrl Pts',(1.08870385957678,-11.4879422226462,10.9923037050953));
#10648=CARTESIAN_POINT('Ctrl Pts',(0.984799940287087,-11.4958808036504,
11.1437012818572));
#10649=CARTESIAN_POINT('Ctrl Pts',(0.745307953378954,-11.5115497231097,
11.3827868553843));
#10650=CARTESIAN_POINT('Ctrl Pts',(0.593674652448182,-11.5202944277784,
11.4864503548939));
#10651=CARTESIAN_POINT('Ctrl Pts',(0.26139245106881,-11.5327733929255,11.6239637415438));
#10652=CARTESIAN_POINT('Ctrl Pts',(0.0807330514364638,-11.5362972391425,
11.6578072726059));
#10653=CARTESIAN_POINT('Ctrl Pts',(-0.0886968229780931,-11.5362972391425,
11.6578072726059));
#10654=CARTESIAN_POINT('Origin',(-0.0886968229780924,16.2000012057142,10.3078072726059));
#10655=CARTESIAN_POINT('',(-0.088696822977779,11.5834283258775,8.95780727260271));
#10656=CARTESIAN_POINT('',(-0.0886968229780923,11.5362996505709,11.6578072726059));
#10657=CARTESIAN_POINT('Ctrl Pts',(-0.0886968229780926,11.5834283258771,
8.95780727260587));
#10658=CARTESIAN_POINT('Ctrl Pts',(-0.258665959021165,11.5834283258771,
8.95780727260587));
#10659=CARTESIAN_POINT('Ctrl Pts',(-0.439810200113418,11.5787106099761,
8.99186624382722));
#10660=CARTESIAN_POINT('Ctrl Pts',(-0.772719647754746,11.5614038817192,
9.13005765427303));
#10661=CARTESIAN_POINT('Ctrl Pts',(-0.924500341537123,11.5490255791854,
9.23417909181128));
#10662=CARTESIAN_POINT('Ctrl Pts',(-1.16405939063838,11.5249794040906,9.47422697160051));
#10663=CARTESIAN_POINT('Ctrl Pts',(-1.26785312558251,11.5117363226006,9.6262165078671));
#10664=CARTESIAN_POINT('Ctrl Pts',(-1.40534901915338,11.4909684308019,9.95937865043048));
#10665=CARTESIAN_POINT('Ctrl Pts',(-1.43904053671719,11.4836634203839,10.1405693130855));
#10666=CARTESIAN_POINT('Ctrl Pts',(-1.43834888045985,11.4777814017933,10.4798716492407));
#10667=CARTESIAN_POINT('Ctrl Pts',(-1.40417808237572,11.4787844778321,10.6603931046871));
#10668=CARTESIAN_POINT('Ctrl Pts',(-1.26609750553296,11.4879446340746,10.9923037050953));
#10669=CARTESIAN_POINT('Ctrl Pts',(-1.16219358624327,11.4958832150788,11.1437012818572));
#10670=CARTESIAN_POINT('Ctrl Pts',(-0.922701599335138,11.5115521345381,
11.3827868553843));
#10671=CARTESIAN_POINT('Ctrl Pts',(-0.771068298404366,11.5202968392069,
11.4864503548939));
#10672=CARTESIAN_POINT('Ctrl Pts',(-0.438786097024993,11.5327758043539,
11.6239637415438));
#10673=CARTESIAN_POINT('Ctrl Pts',(-0.258126697392649,11.5362996505709,
11.6578072726059));
#10674=CARTESIAN_POINT('Ctrl Pts',(-0.088696822978092,11.5362996505709,
11.6578072726059));
#10675=CARTESIAN_POINT('',(-0.0886968229780925,6.7500012057142,11.6578072726059));
#10676=CARTESIAN_POINT('',(-0.0886968229780925,16.2000012057142,11.6578072726059));
#10677=CARTESIAN_POINT('Origin',(-0.0886968229780924,6.7500012057142,10.3078072726059));
#10678=CARTESIAN_POINT('Ctrl Pts',(-0.0886968229780922,11.5362996505709,
11.6578072726059));
#10679=CARTESIAN_POINT('Ctrl Pts',(0.0807330514364649,11.5362996505709,
11.6578072726059));
#10680=CARTESIAN_POINT('Ctrl Pts',(0.26139245106881,11.5327758043539,11.6239637415438));
#10681=CARTESIAN_POINT('Ctrl Pts',(0.593674652448182,11.5202968392069,11.4864503548939));
#10682=CARTESIAN_POINT('Ctrl Pts',(0.745307953378954,11.5115521345381,11.3827868553843));
#10683=CARTESIAN_POINT('Ctrl Pts',(0.984799940287087,11.4958832150788,11.1437012818572));
#10684=CARTESIAN_POINT('Ctrl Pts',(1.08870385957678,11.4879446340746,10.9923037050953));
#10685=CARTESIAN_POINT('Ctrl Pts',(1.22678443641954,11.4787844778321,10.6603931046871));
#10686=CARTESIAN_POINT('Ctrl Pts',(1.26095523450366,11.4777814017933,10.4798716492407));
#10687=CARTESIAN_POINT('Ctrl Pts',(1.26130037217385,11.4807165392562,10.3105591959141));
#10688=CARTESIAN_POINT('Ctrl Pts',(1.261646890761,11.4836634203839,10.1405693130855));
#10689=CARTESIAN_POINT('Ctrl Pts',(1.22795537319719,11.4909684308019,9.95937865043048));
#10690=CARTESIAN_POINT('Ctrl Pts',(1.09045947962633,11.5117363226006,9.6262165078671));
#10691=CARTESIAN_POINT('Ctrl Pts',(0.986665744682193,11.5249794040906,9.47422697160051));
#10692=CARTESIAN_POINT('Ctrl Pts',(0.747106695580938,11.5490255791854,9.23417909181128));
#10693=CARTESIAN_POINT('Ctrl Pts',(0.595326001798561,11.5614038817192,9.13005765427303));
#10694=CARTESIAN_POINT('Ctrl Pts',(0.262416554157233,11.5787106099761,8.99186624382722));
#10695=CARTESIAN_POINT('Ctrl Pts',(0.0812723130649793,11.5834283258771,
8.95780727260587));
#10696=CARTESIAN_POINT('Ctrl Pts',(-0.0886968229780928,11.5834283258771,
8.95780727260587));
#10697=CARTESIAN_POINT('Origin',(-0.0886968229780924,1.20571420388653E-6,
2.2793514595497));
#10698=CARTESIAN_POINT('',(9.15430644803649,-6.7499987942858,16.869309255546));
#10699=CARTESIAN_POINT('',(9.15430644803649,6.7500012057142,16.8693092555461));
#10700=CARTESIAN_POINT('Origin',(-0.0886968229780924,1.20571420052696E-6,
16.869309255546));
#10701=CARTESIAN_POINT('',(9.21661950459473,6.7500012057142,13.9829593621724));
#10702=CARTESIAN_POINT('Ctrl Pts',(9.21661950459473,6.7500012057142,13.9829593621724));
#10703=CARTESIAN_POINT('Ctrl Pts',(9.19587255806943,6.7500012057142,14.9450765126902));
#10704=CARTESIAN_POINT('Ctrl Pts',(9.17510170146439,6.7500012057142,15.9071931479242));
#10705=CARTESIAN_POINT('Ctrl Pts',(9.15430644803649,6.7500012057142,16.8693092555461));
#10706=CARTESIAN_POINT('',(3.79009320173104,10.9021010231549,9.63818989051917));
#10707=CARTESIAN_POINT('Ctrl Pts',(3.79009320173104,10.9021010231549,9.63818989051917));
#10708=CARTESIAN_POINT('Ctrl Pts',(4.20613537995868,10.7443331834893,10.1642783227575));
#10709=CARTESIAN_POINT('Ctrl Pts',(4.64694412836354,10.5510444035147,10.650798216911));
#10710=CARTESIAN_POINT('Ctrl Pts',(5.63962932833512,10.0329253784985,11.623427806388));
#10711=CARTESIAN_POINT('Ctrl Pts',(6.25376498977623,9.65635758742349,12.1401590568172));
#10712=CARTESIAN_POINT('Ctrl Pts',(7.45983969473753,8.72586417187042,13.0128149073975));
#10713=CARTESIAN_POINT('Ctrl Pts',(8.04927182637234,8.17020873374597,13.3703563763539));
#10714=CARTESIAN_POINT('Ctrl Pts',(8.77823970806682,7.33062511965669,13.765805640045));
#10715=CARTESIAN_POINT('Ctrl Pts',(9.0022731985786,7.04855860769825,13.8797875988384));
#10716=CARTESIAN_POINT('Ctrl Pts',(9.21661950459473,6.7500012057142,13.9829593621724));
#10717=CARTESIAN_POINT('',(-2.04522493875568,11.4685794314074,6.04489666046755));
#10718=CARTESIAN_POINT('Ctrl Pts',(3.79009320173104,10.9021010231549,9.63818989051918));
#10719=CARTESIAN_POINT('Ctrl Pts',(3.58403350493312,10.9802411611199,9.37762586958811));
#10720=CARTESIAN_POINT('Ctrl Pts',(3.36708944887808,11.0552744978014,9.13007814566772));
#10721=CARTESIAN_POINT('Ctrl Pts',(2.72899476230882,11.2526099540629,8.46885648760705));
#10722=CARTESIAN_POINT('Ctrl Pts',(2.23455214075372,11.3774728044186,8.03794303289295));
#10723=CARTESIAN_POINT('Ctrl Pts',(1.16082935689865,11.55806672261,7.28307730157583));
#10724=CARTESIAN_POINT('Ctrl Pts',(0.581234136539683,11.6122856652571,6.9592121964347));
#10725=CARTESIAN_POINT('Ctrl Pts',(-0.617178694535791,11.6334215213611,
6.42377887019057));
#10726=CARTESIAN_POINT('Ctrl Pts',(-1.32470976378382,11.5888829746167,6.19261208415742));
#10727=CARTESIAN_POINT('Ctrl Pts',(-2.04522493875569,11.4685794314074,6.04489666046755));
#10728=CARTESIAN_POINT('',(-11.0841037493982,3.97811118728989,2.68507615460814));
#10729=CARTESIAN_POINT('Ctrl Pts',(-11.0841037493982,3.97811118728989,2.68507615460814));
#10730=CARTESIAN_POINT('Ctrl Pts',(-11.0229709537136,4.14532830143922,2.71923525419231));
#10731=CARTESIAN_POINT('Ctrl Pts',(-10.9580372989578,4.31099505858238,2.75525104909031));
#10732=CARTESIAN_POINT('Ctrl Pts',(-10.2946364808206,5.8956035577366,3.11981222038323));
#10733=CARTESIAN_POINT('Ctrl Pts',(-9.4105044355921,7.17556183564993,3.57669501792371));
#10734=CARTESIAN_POINT('Ctrl Pts',(-7.37826383459281,9.21886256467337,4.47105415851211));
#10735=CARTESIAN_POINT('Ctrl Pts',(-6.07582291747799,10.1190258596251,4.97344565700631));
#10736=CARTESIAN_POINT('Ctrl Pts',(-3.8030697228604,11.0693349098104,5.64394863077188));
#10737=CARTESIAN_POINT('Ctrl Pts',(-2.92780373849181,11.3212163217078,5.8639559865285));
#10738=CARTESIAN_POINT('Ctrl Pts',(-2.04522493875568,11.4685794314074,6.04489666046755));
#10739=CARTESIAN_POINT('',(-10.9838133703314,3.97811209444304,8.08507411790788));
#10740=CARTESIAN_POINT('Ctrl Pts',(-11.0841054060657,3.97811209444304,2.68507522891397));
#10741=CARTESIAN_POINT('Ctrl Pts',(-11.0671368467592,3.97811209444304,3.59910749288785));
#10742=CARTESIAN_POINT('Ctrl Pts',(-11.0501656900449,3.97811209444304,4.51314082004822));
#10743=CARTESIAN_POINT('Ctrl Pts',(-11.0331899258266,3.97811209444304,5.42717406162499));
#10744=CARTESIAN_POINT('Ctrl Pts',(-11.0167354225938,3.97811209444304,6.31314082783784));
#10745=CARTESIAN_POINT('Ctrl Pts',(-11.0002765904705,3.97811209444304,7.1991075136423));
#10746=CARTESIAN_POINT('Ctrl Pts',(-10.9838133703314,3.97811209444304,8.08507411790788));
#10747=CARTESIAN_POINT('',(-11.6873575570212,1.20571420530696E-6,8.08507411790788));
#10748=CARTESIAN_POINT('Origin',(-0.0886968229780924,1.20571420388653E-6,
8.08507411790788));
#10749=CARTESIAN_POINT('',(-11.2742087842189,1.20571420492242E-6,31.7543514595497));
#10750=CARTESIAN_POINT('',(-11.7886968229781,1.20571420531937E-6,2.2793514595497));
#10751=CARTESIAN_POINT('',(11.096827150046,1.20571420194828E-6,31.7536633049461));
#10752=CARTESIAN_POINT('Ctrl Pts',(-11.2742087842189,1.20571420458848E-6,
31.7543514595497));
#10753=CARTESIAN_POINT('Ctrl Pts',(-11.2742087842189,0.714879232030262,
31.7543514595497));
#10754=CARTESIAN_POINT('Ctrl Pts',(-11.2039243099315,1.44919356167399,31.793099916814));
#10755=CARTESIAN_POINT('Ctrl Pts',(-10.9133728006453,2.90079942562337,31.9472948843815));
#10756=CARTESIAN_POINT('Ctrl Pts',(-10.6932214582039,3.61814006950708,32.0624969509637));
#10757=CARTESIAN_POINT('Ctrl Pts',(-9.82880176569562,5.67152012999344,32.4870523054472));
#10758=CARTESIAN_POINT('Ctrl Pts',(-8.96991780652531,6.90812806220324,32.8751111589287));
#10759=CARTESIAN_POINT('Ctrl Pts',(-7.00675772315132,8.85727351788031,33.5789580196972));
#10760=CARTESIAN_POINT('Ctrl Pts',(-5.76477228566963,9.70843557232902,33.9447939157601));
#10761=CARTESIAN_POINT('Ctrl Pts',(-3.01891541115682,10.8482984598267,34.4584272670688));
#10762=CARTESIAN_POINT('Ctrl Pts',(-1.51351007601002,11.1358317415463,34.6005984149743));
#10763=CARTESIAN_POINT('Ctrl Pts',(1.33613242402791,11.1358330727219,34.6005221519735));
#10764=CARTESIAN_POINT('Ctrl Pts',(2.84154593721425,10.8482953636761,34.4582674767084));
#10765=CARTESIAN_POINT('Ctrl Pts',(5.58740871904998,9.70842501571461,33.9444749141113));
#10766=CARTESIAN_POINT('Ctrl Pts',(6.82939227785914,8.85726022067858,33.578563036809));
#10767=CARTESIAN_POINT('Ctrl Pts',(8.79254166028598,6.90811816343161,32.8745913568126));
#10768=CARTESIAN_POINT('Ctrl Pts',(9.65142087432493,5.67151703383353,32.4864738899089));
#10769=CARTESIAN_POINT('Ctrl Pts',(10.5158385377037,3.61814283629084,32.0618549656255));
#10770=CARTESIAN_POINT('Ctrl Pts',(10.7359899995928,2.90080333450706,31.9466357770987));
#10771=CARTESIAN_POINT('Ctrl Pts',(11.0265421577798,1.44919736945254,31.7924176982799));
#10772=CARTESIAN_POINT('Ctrl Pts',(11.096827150046,0.714881784716172,31.7536633049461));
#10773=CARTESIAN_POINT('Ctrl Pts',(11.096827150046,1.20571420431093E-6,
31.7536633049461));
#10774=CARTESIAN_POINT('Ctrl Pts',(11.096827150046,1.20571420389459E-6,
31.7536633049461));
#10775=CARTESIAN_POINT('Ctrl Pts',(11.096827150046,-0.714879373287764,31.7536633049461));
#10776=CARTESIAN_POINT('Ctrl Pts',(11.0265421577798,-1.44919495802413,31.7924176982799));
#10777=CARTESIAN_POINT('Ctrl Pts',(10.7359899995928,-2.90080092307865,31.9466357770987));
#10778=CARTESIAN_POINT('Ctrl Pts',(10.5158385377037,-3.61814042486243,32.0618549656255));
#10779=CARTESIAN_POINT('Ctrl Pts',(9.65142087432494,-5.67151462240512,32.4864738899089));
#10780=CARTESIAN_POINT('Ctrl Pts',(8.79254166028598,-6.9081157520032,32.8745913568126));
#10781=CARTESIAN_POINT('Ctrl Pts',(6.82939227785914,-8.85725780925017,33.578563036809));
#10782=CARTESIAN_POINT('Ctrl Pts',(5.58740871904998,-9.70842260428621,33.9444749141113));
#10783=CARTESIAN_POINT('Ctrl Pts',(2.84154593721424,-10.8482929522477,34.4582674767085));
#10784=CARTESIAN_POINT('Ctrl Pts',(1.33613242402791,-11.1358306612935,34.6005221519735));
#10785=CARTESIAN_POINT('Ctrl Pts',(-1.51351007601001,-11.1358293301179,
34.6005984149743));
#10786=CARTESIAN_POINT('Ctrl Pts',(-3.01891541115682,-10.8482960483983,
34.4584272670688));
#10787=CARTESIAN_POINT('Ctrl Pts',(-5.76477228566962,-9.70843316090061,
33.9447939157601));
#10788=CARTESIAN_POINT('Ctrl Pts',(-7.00675772315132,-8.85727110645191,
33.5789580196972));
#10789=CARTESIAN_POINT('Ctrl Pts',(-8.96991780652531,-6.90812565077484,
32.8751111589287));
#10790=CARTESIAN_POINT('Ctrl Pts',(-9.82880176569561,-5.67151771856503,
32.4870523054472));
#10791=CARTESIAN_POINT('Ctrl Pts',(-10.6932214582039,-3.61813765807868,
32.0624969509637));
#10792=CARTESIAN_POINT('Ctrl Pts',(-10.9133728006453,-2.90079701419497,
31.9472948843814));
#10793=CARTESIAN_POINT('Ctrl Pts',(-11.2039243099315,-1.44919115024558,
31.793099916814));
#10794=CARTESIAN_POINT('Ctrl Pts',(-11.2742087842189,-0.714876820601855,
31.7543514595497));
#10795=CARTESIAN_POINT('Ctrl Pts',(-11.2742087842189,1.20571420417215E-6,
31.7543514595497));
#10796=CARTESIAN_POINT('',(-10.9838133703314,-3.97810968301463,8.08507411790788));
#10797=CARTESIAN_POINT('Origin',(-0.0886968229780924,1.20571420388653E-6,
8.08507411790788));
#10798=CARTESIAN_POINT('',(-11.084104180594,-3.97810913882278,2.68507514951319));
#10799=CARTESIAN_POINT('Ctrl Pts',(-10.9838133703314,-3.97810968301463,
8.08507411790788));
#10800=CARTESIAN_POINT('Ctrl Pts',(-11.0002765904705,-3.97810968301463,
7.19910751364231));
#10801=CARTESIAN_POINT('Ctrl Pts',(-11.016735422596,-3.97810968301463,6.31314082782715));
#10802=CARTESIAN_POINT('Ctrl Pts',(-11.0331899258289,-3.97810968301463,
5.42717406161412));
#10803=CARTESIAN_POINT('Ctrl Pts',(-11.0501656900472,-3.97810968301463,
4.51314082003718));
#10804=CARTESIAN_POINT('Ctrl Pts',(-11.0671368467592,-3.97810968301463,
3.59910749288785));
#10805=CARTESIAN_POINT('Ctrl Pts',(-11.0841054060657,-3.97810968301463,
2.68507522891397));
#10806=CARTESIAN_POINT('',(-2.04522493875568,-11.468577019979,6.04489666046755));
#10807=CARTESIAN_POINT('Ctrl Pts',(-2.04522493875568,-11.468577019979,6.04489666046755));
#10808=CARTESIAN_POINT('Ctrl Pts',(-2.92780373849181,-11.3212139102794,
5.8639559865285));
#10809=CARTESIAN_POINT('Ctrl Pts',(-3.8030697228604,-11.069332498382,5.64394863077188));
#10810=CARTESIAN_POINT('Ctrl Pts',(-6.07582291747798,-10.1190234481967,
4.97344565700631));
#10811=CARTESIAN_POINT('Ctrl Pts',(-7.3782638345928,-9.21886015324496,4.47105415851212));
#10812=CARTESIAN_POINT('Ctrl Pts',(-9.4105044355921,-7.17555942422152,3.57669501792372));
#10813=CARTESIAN_POINT('Ctrl Pts',(-10.2946364808206,-5.89560114630819,
3.11981222038324));
#10814=CARTESIAN_POINT('Ctrl Pts',(-10.9580372989578,-4.31099264715397,
2.75525104909032));
#10815=CARTESIAN_POINT('Ctrl Pts',(-11.0229709537136,-4.14532589001081,
2.71923525419232));
#10816=CARTESIAN_POINT('Ctrl Pts',(-11.0841037493982,-3.97810877586148,
2.68507615460814));
#10817=CARTESIAN_POINT('',(3.79009320173104,-10.9020986117265,9.63818989051917));
#10818=CARTESIAN_POINT('Ctrl Pts',(-2.04522493875568,-11.468577019979,6.04489666046755));
#10819=CARTESIAN_POINT('Ctrl Pts',(-1.32470976378382,-11.5888805631882,
6.19261208415742));
#10820=CARTESIAN_POINT('Ctrl Pts',(-0.617178694535787,-11.6334191099327,
6.42377887019057));
#10821=CARTESIAN_POINT('Ctrl Pts',(0.581234136539686,-11.6122832538287,
6.95921219643471));
#10822=CARTESIAN_POINT('Ctrl Pts',(1.16082935689865,-11.5580643111816,7.28307730157583));
#10823=CARTESIAN_POINT('Ctrl Pts',(2.23455214075372,-11.3774703929902,8.03794303289295));
#10824=CARTESIAN_POINT('Ctrl Pts',(2.72899476230882,-11.2526075426344,8.46885648760705));
#10825=CARTESIAN_POINT('Ctrl Pts',(3.36708944887808,-11.055272086373,9.13007814566771));
#10826=CARTESIAN_POINT('Ctrl Pts',(3.58403350493311,-10.9802387496915,9.37762586958811));
#10827=CARTESIAN_POINT('Ctrl Pts',(3.79009320173103,-10.9020986117265,9.63818989051917));
#10828=CARTESIAN_POINT('',(9.21661950459473,-6.7499987942858,13.9829593621724));
#10829=CARTESIAN_POINT('Ctrl Pts',(9.21661950459473,-6.74999879428579,13.9829593621724));
#10830=CARTESIAN_POINT('Ctrl Pts',(9.0022731985786,-7.04855619626984,13.8797875988384));
#10831=CARTESIAN_POINT('Ctrl Pts',(8.77823970806681,-7.33062270822828,13.765805640045));
#10832=CARTESIAN_POINT('Ctrl Pts',(8.04927182637234,-8.17020632231756,13.3703563763539));
#10833=CARTESIAN_POINT('Ctrl Pts',(7.45983969473753,-8.72586176044201,13.0128149073975));
#10834=CARTESIAN_POINT('Ctrl Pts',(6.25376498977623,-9.65635517599508,12.1401590568172));
#10835=CARTESIAN_POINT('Ctrl Pts',(5.63962932833512,-10.0329229670701,11.623427806388));
#10836=CARTESIAN_POINT('Ctrl Pts',(4.64694412836354,-10.5510419920863,10.650798216911));
#10837=CARTESIAN_POINT('Ctrl Pts',(4.20613537995868,-10.7443307720609,10.1642783227575));
#10838=CARTESIAN_POINT('Ctrl Pts',(3.79009320173104,-10.9020986117265,9.63818989051917));
#10839=CARTESIAN_POINT('Ctrl Pts',(9.15430644803649,-6.7499987942858,16.869309255546));
#10840=CARTESIAN_POINT('Ctrl Pts',(9.17510170146438,-6.7499987942858,15.9071931479241));
#10841=CARTESIAN_POINT('Ctrl Pts',(9.19587255806942,-6.7499987942858,14.9450765126902));
#10842=CARTESIAN_POINT('Ctrl Pts',(9.21661950459473,-6.7499987942858,13.9829593621724));
#10843=CARTESIAN_POINT('Origin',(4.28112241113661,32.4000012057142,-24.8132842517073));
#10844=CARTESIAN_POINT('',(-7.28869682297809,-6.7499987942858,4.48499697586492));
#10845=CARTESIAN_POINT('',(-2.04522493875568,-6.7499987942858,6.04489666046755));
#10846=CARTESIAN_POINT('Origin',(4.28112241113661,-6.7499987942858,-24.8132842517073));
#10847=CARTESIAN_POINT('',(-2.04522493875568,32.4000012057142,6.04489666046755));
#10848=CARTESIAN_POINT('Ctrl Pts',(-11.0841037493982,-3.97810877586148,
2.68507615460814));
#10849=CARTESIAN_POINT('Ctrl Pts',(-11.2880488632369,-3.42025577733562,
2.57111798575136));
#10850=CARTESIAN_POINT('Ctrl Pts',(-11.4494008749826,-2.8449890145717,2.47808040767037));
#10851=CARTESIAN_POINT('Ctrl Pts',(-11.7156745135564,-1.50931079877612,
2.32309001764736));
#10852=CARTESIAN_POINT('Ctrl Pts',(-11.7886968229781,-0.744842394221963,
2.2793514595497));
#10853=CARTESIAN_POINT('Ctrl Pts',(-11.7886968229781,0.744844805650374,
2.2793514595497));
#10854=CARTESIAN_POINT('Ctrl Pts',(-11.7156745135564,1.50931321020453,2.32309001764737));
#10855=CARTESIAN_POINT('Ctrl Pts',(-11.4494008749826,2.84499142600011,2.47808040767037));
#10856=CARTESIAN_POINT('Ctrl Pts',(-11.2880488632369,3.42025818876404,2.57111798575136));
#10857=CARTESIAN_POINT('Ctrl Pts',(-11.0841037493982,3.97811118728989,2.68507615460815));
#10858=CARTESIAN_POINT('',(-2.04522493875568,6.7500012057142,6.04489666046755));
#10859=CARTESIAN_POINT('',(-2.04522493875568,32.4000012057142,6.04489666046755));
#10860=CARTESIAN_POINT('',(-7.28869682297809,6.7500012057142,4.48499697586491));
#10861=CARTESIAN_POINT('Origin',(4.28112241113661,6.75000120571421,-24.8132842517073));
#10862=CARTESIAN_POINT('',(-7.28869682297809,32.4000012057142,4.48499697586492));
#10863=CARTESIAN_POINT('Origin',(-10.1906081922044,1.20571420388653E-6,
-7.82255990967661));
#10864=CARTESIAN_POINT('',(-16.8798656013815,-3.97810968301463,-1.13330250049948));
#10865=CARTESIAN_POINT('',(-18.3070733952457,-3.97810968301463,0.293905293364732));
#10866=CARTESIAN_POINT('',(-16.2434694983136,-3.97810968301463,-1.76969860356737));
#10867=CARTESIAN_POINT('',(-18.3070733952457,-2.2499987942858,0.293905293364733));
#10868=CARTESIAN_POINT('',(-18.3070733952457,-2.2499987942858,0.293905293364733));
#10869=CARTESIAN_POINT('',(-16.8798656013815,-2.2499987942858,-1.13330250049948));
#10870=CARTESIAN_POINT('',(-10.1906081922044,-2.2499987942858,-7.82255990967661));
#10871=CARTESIAN_POINT('',(-16.8798656013815,-3.97810968301463,-1.13330250049948));
#10872=CARTESIAN_POINT('Origin',(-0.0886968229780924,1.20571420388653E-6,
2.2793514595497));
#10873=CARTESIAN_POINT('Origin',(-0.0886968229780924,1.20571420388653E-6,
2.68507411790788));
#10874=CARTESIAN_POINT('Origin',(-0.0893230609073105,32.4000012057142,11.2005602920677));
#10875=CARTESIAN_POINT('',(6.61050363813806,-3.97810968301463,33.6209153785234));
#10876=CARTESIAN_POINT('',(6.61050363813806,3.97811209444304,33.6209153785234));
#10877=CARTESIAN_POINT('',(6.61050363813806,32.4000012057142,33.6209153785234));
#10878=CARTESIAN_POINT('',(-6.78789728409425,-3.97810968301463,33.621289615095));
#10879=CARTESIAN_POINT('Origin',(-0.0893230609073105,-3.97810968301463,
11.2005602920677));
#10880=CARTESIAN_POINT('',(-6.78789728409425,3.97811209444304,33.621289615095));
#10881=CARTESIAN_POINT('',(-6.78789728409425,32.4000012057142,33.621289615095));
#10882=CARTESIAN_POINT('Origin',(-0.0893230609073105,3.97811209444304,11.2005602920677));
#10883=CARTESIAN_POINT('Origin',(14.3113031770219,6.7500012057142,14.8344044426714));
#10884=CARTESIAN_POINT('',(6.51868832412356,6.7500012057142,14.8344044426714));
#10885=CARTESIAN_POINT('',(6.51868832412356,-6.7499987942858,14.8344044426714));
#10886=CARTESIAN_POINT('Origin',(-0.0886968229780924,1.20571420076229E-6,
14.8344044426714));
#10887=CARTESIAN_POINT('',(-7.28869682297809,-6.7499987942858,14.8344044426714));
#10888=CARTESIAN_POINT('',(14.3113031770219,-6.7499987942858,14.8344044426714));
#10889=CARTESIAN_POINT('',(-7.28869682297809,6.7500012057142,14.8344044426714));
#10890=CARTESIAN_POINT('',(-7.28869682297809,6.7500012057142,14.8344044426714));
#10891=CARTESIAN_POINT('',(14.3113031770219,6.7500012057142,14.8344044426714));
#10892=CARTESIAN_POINT('Origin',(14.3113031770219,-6.7499987942858,-10.275701523572));
#10893=CARTESIAN_POINT('',(3.79009320173104,-6.74999879428579,9.63818989051917));
#10894=CARTESIAN_POINT('Origin',(15.9282673556341,-6.74999879428579,0.0390576814896602));
#10895=CARTESIAN_POINT('Origin',(-4.05358917681673,-6.7499987942858,15.8411445690945));
#10896=CARTESIAN_POINT('',(-7.28869682297809,-6.7499987942858,-10.275701523572));
#10897=CARTESIAN_POINT('Ctrl Pts',(6.51868832412356,-6.7499987942858,14.8344044426714));
#10898=CARTESIAN_POINT('Ctrl Pts',(6.89318504201329,-6.7499987942858,14.8344044426714));
#10899=CARTESIAN_POINT('Ctrl Pts',(7.33776310853797,-6.7499987942858,14.9000334212391));
#10900=CARTESIAN_POINT('Ctrl Pts',(7.97286532132927,-6.7499987942858,15.1264890486251));
#10901=CARTESIAN_POINT('Ctrl Pts',(8.28752674897206,-6.7499987942858,15.3008175202491));
#10902=CARTESIAN_POINT('Ctrl Pts',(8.70384046495954,-6.7499987942858,15.665664492641));
#10903=CARTESIAN_POINT('Ctrl Pts',(8.89134878165894,-6.7499987942858,15.9056447643772));
#10904=CARTESIAN_POINT('Ctrl Pts',(9.09386350816702,-6.7499987942858,16.3417623265294));
#10905=CARTESIAN_POINT('Ctrl Pts',(9.15468363432064,-6.7499987942858,16.6073512291574));
#10906=CARTESIAN_POINT('Ctrl Pts',(9.15468363432064,-6.7499987942858,16.8344044426714));
#10907=CARTESIAN_POINT('Ctrl Pts',(9.15468363432064,-6.7499987942858,16.8459433493969));
#10908=CARTESIAN_POINT('Ctrl Pts',(9.15455990443804,-6.7499987942858,16.8575828061736));
#10909=CARTESIAN_POINT('Ctrl Pts',(9.15430644803649,-6.7499987942858,16.869309255546));
#10910=CARTESIAN_POINT('Origin',(14.3113031770219,6.7500012057142,-10.275701523572));
#10911=CARTESIAN_POINT('',(3.79009320173104,6.7500012057142,9.63818989051917));
#10912=CARTESIAN_POINT('Origin',(-4.05358917681673,6.7500012057142,15.8411445690945));
#10913=CARTESIAN_POINT('Origin',(15.9282673556341,6.7500012057142,0.0390576814896602));
#10914=CARTESIAN_POINT('Ctrl Pts',(9.15430644803649,6.7500012057142,16.8693092555461));
#10915=CARTESIAN_POINT('Ctrl Pts',(9.1545597299,6.7500012057142,16.8575908813751));
#10916=CARTESIAN_POINT('Ctrl Pts',(9.15468363432064,6.7500012057142,16.8459519530649));
#10917=CARTESIAN_POINT('Ctrl Pts',(9.15468363432064,6.7500012057142,16.8344044426714));
#10918=CARTESIAN_POINT('Ctrl Pts',(9.15468363432064,6.7500012057142,16.6073512291574));
#10919=CARTESIAN_POINT('Ctrl Pts',(9.09386350816702,6.7500012057142,16.3417623265294));
#10920=CARTESIAN_POINT('Ctrl Pts',(8.89134878165894,6.7500012057142,15.9056447643772));
#10921=CARTESIAN_POINT('Ctrl Pts',(8.70384046495954,6.7500012057142,15.665664492641));
#10922=CARTESIAN_POINT('Ctrl Pts',(8.28752674897205,6.7500012057142,15.3008175202491));
#10923=CARTESIAN_POINT('Ctrl Pts',(7.97286532132927,6.7500012057142,15.126489048625));
#10924=CARTESIAN_POINT('Ctrl Pts',(7.33776310853796,6.7500012057142,14.9000334212391));
#10925=CARTESIAN_POINT('Ctrl Pts',(6.89318504201329,6.7500012057142,14.8344044426714));
#10926=CARTESIAN_POINT('Ctrl Pts',(6.51868832412356,6.7500012057142,14.8344044426714));
#10927=CARTESIAN_POINT('',(-7.28869682297809,6.7500012057142,-10.275701523572));
#10928=CARTESIAN_POINT('Origin',(-7.28869682297809,1.20571420388653E-6,
2.2793514595497));
#10929=CARTESIAN_POINT('Origin',(11.8416209672313,-3.97810968301463,2.68507411790788));
#10930=CARTESIAN_POINT('',(-11.7886967768384,-3.97810968301463,2.68507411790788));
#10931=CARTESIAN_POINT('',(11.8416209672313,-3.97810968301463,2.68507411790788));
#10932=CARTESIAN_POINT('',(-11.7886967768384,3.97811209444304,2.68507411790788));
#10933=CARTESIAN_POINT('',(-11.7886967768384,-3.97810968301463,2.68507411790788));
#10934=CARTESIAN_POINT('',(11.8416209672313,3.97811209444304,2.68507411790788));
#10935=CARTESIAN_POINT('Origin',(11.8416209672313,3.97811209444304,8.08507411790788));
#10936=CARTESIAN_POINT('',(-18.3070733952457,3.97811209444304,0.293905293364732));
#10937=CARTESIAN_POINT('',(-16.8798656013815,3.97811209444304,-1.13330250049948));
#10938=CARTESIAN_POINT('',(-18.9434694983136,3.97811209444304,0.930301396432627));
#10939=CARTESIAN_POINT('',(-18.3070733952457,3.97811209444304,1.56669749950052));
#10940=CARTESIAN_POINT('Origin',(-17.6706772921778,3.97811209444304,0.930301396432626));
#10941=CARTESIAN_POINT('',(-11.7886967768384,3.97811209444304,8.08507411790788));
#10942=CARTESIAN_POINT('',(-18.9434694983136,3.97811209444304,0.930301396432627));
#10943=CARTESIAN_POINT('',(11.8416209672313,3.97811209444304,8.08507411790788));
#10944=CARTESIAN_POINT('',(-15.6070733952457,3.97811209444304,-1.13330250049948));
#10945=CARTESIAN_POINT('',(-16.2434694983136,3.97811209444304,-1.76969860356737));
#10946=CARTESIAN_POINT('Origin',(-16.2434694983136,3.97811209444304,-0.496906397431586));
#10947=CARTESIAN_POINT('Origin',(11.8416209672313,-3.97810968301463,8.08507411790788));
#10948=CARTESIAN_POINT('',(-11.7886967768384,-3.97810968301463,8.08507411790788));
#10949=CARTESIAN_POINT('',(-11.7886967768384,-3.97810968301463,8.08507411790788));
#10950=CARTESIAN_POINT('',(11.8416209672313,-3.97810968301463,8.08507411790788));
#10951=CARTESIAN_POINT('Origin',(11.8416209672313,-3.97810968301463,8.08507411790788));
#10952=CARTESIAN_POINT('',(-18.3070733952457,-3.97810968301463,1.56669749950052));
#10953=CARTESIAN_POINT('',(-18.9434694983136,-3.97810968301463,0.930301396432627));
#10954=CARTESIAN_POINT('Origin',(-17.6706772921778,-3.97810968301463,0.930301396432626));
#10955=CARTESIAN_POINT('',(-15.6070733952457,-3.97810968301463,-1.13330250049948));
#10956=CARTESIAN_POINT('Origin',(-16.2434694983136,-3.97810968301463,-0.496906397431586));
#10957=CARTESIAN_POINT('',(-16.2434694983136,-3.97810968301463,-1.76969860356737));
#10958=CARTESIAN_POINT('Origin',(-16.2434694983136,3.97811209444304,-1.76969860356737));
#10959=CARTESIAN_POINT('',(-15.6070733952457,-2.2499987942858,-1.13330250049948));
#10960=CARTESIAN_POINT('',(-15.6070733952457,-2.2499987942858,-1.13330250049948));
#10961=CARTESIAN_POINT('',(-12.4250928799063,-2.2499987942858,2.04867801483998));
#10962=CARTESIAN_POINT('',(-16.2434694983136,-2.2499987942858,-1.76969860356737));
#10963=CARTESIAN_POINT('',(-12.4250928799063,2.2500012057142,2.04867801483998));
#10964=CARTESIAN_POINT('',(-12.4250928799063,3.97811209444304,2.04867801483998));
#10965=CARTESIAN_POINT('',(-15.6070733952457,2.2500012057142,-1.13330250049948));
#10966=CARTESIAN_POINT('',(-16.2434694983136,2.2500012057142,-1.76969860356737));
#10967=CARTESIAN_POINT('',(-15.6070733952457,3.97811209444304,-1.13330250049948));
#10968=CARTESIAN_POINT('Origin',(-18.9434694983136,-3.97810968301463,0.930301396432627));
#10969=CARTESIAN_POINT('',(-15.1250928799063,2.2500012057142,4.74867801483998));
#10970=CARTESIAN_POINT('',(-18.3070733952457,2.2500012057142,1.56669749950052));
#10971=CARTESIAN_POINT('',(-22.1254500136531,2.2500012057142,-2.25167911890684));
#10972=CARTESIAN_POINT('',(-15.1250928799063,-2.2499987942858,4.74867801483998));
#10973=CARTESIAN_POINT('',(-15.1250928799063,-3.97810968301463,4.74867801483998));
#10974=CARTESIAN_POINT('',(-18.3070733952457,-2.2499987942858,1.56669749950052));
#10975=CARTESIAN_POINT('',(-22.1254500136531,-2.2499987942858,-2.25167911890684));
#10976=CARTESIAN_POINT('',(-18.3070733952457,-3.97810968301463,1.56669749950052));
#10977=CARTESIAN_POINT('',(-18.3070733952457,2.2500012057142,1.56669749950052));
#10978=CARTESIAN_POINT('Origin',(-10.1906081922044,1.20571420388653E-6,
-7.82255990967661));
#10979=CARTESIAN_POINT('',(-18.3070733952457,2.2500012057142,0.293905293364733));
#10980=CARTESIAN_POINT('',(-16.8798656013815,2.2500012057142,-1.13330250049948));
#10981=CARTESIAN_POINT('',(-10.1906081922044,2.2500012057142,-7.82255990967661));
#10982=CARTESIAN_POINT('',(-18.3070733952457,3.97811209444304,0.293905293364733));
#10983=CARTESIAN_POINT('',(-16.8798656013815,2.2500012057142,-1.13330250049948));
#10984=CARTESIAN_POINT('Origin',(-11.3067162614989,2.2500012057142,-0.342490809703158));
#10985=CARTESIAN_POINT('',(-13.6978850860421,-2.2499987942858,2.04867801483998));
#10986=CARTESIAN_POINT('',(-15.1250928799063,-2.2499987942858,3.4758858087042));
#10987=CARTESIAN_POINT('',(-11.3067162614989,-2.2499987942858,-0.342490809703158));
#10988=CARTESIAN_POINT('',(-15.1250928799063,2.2500012057142,3.4758858087042));
#10989=CARTESIAN_POINT('',(-15.1250928799063,2.2500012057142,3.4758858087042));
#10990=CARTESIAN_POINT('',(-13.6978850860421,2.2500012057142,2.04867801483998));
#10991=CARTESIAN_POINT('',(-11.3067162614989,2.2500012057142,-0.342490809703158));
#10992=CARTESIAN_POINT('',(-13.6978850860421,2.2500012057142,2.04867801483998));
#10993=CARTESIAN_POINT('Origin',(-17.6706772921778,-2.2499987942858,-6.70645184038209));
#10994=CARTESIAN_POINT('Origin',(-17.6706772921778,-2.2499987942858,0.930301396432626));
#10995=CARTESIAN_POINT('Origin',(-14.4886967768384,-2.2499987942858,4.11228191177209));
#10996=CARTESIAN_POINT('Origin',(-13.0614889829742,-2.2499987942858,2.68507411790788));
#10997=CARTESIAN_POINT('Origin',(-16.2434694983136,-2.2499987942858,-0.496906397431586));
#10998=CARTESIAN_POINT('Origin',(-17.6706772921778,2.2500012057142,-6.70645184038209));
#10999=CARTESIAN_POINT('Origin',(-17.6706772921778,2.2500012057142,0.930301396432626));
#11000=CARTESIAN_POINT('Origin',(-16.2434694983136,2.2500012057142,-0.496906397431586));
#11001=CARTESIAN_POINT('Origin',(-13.0614889829742,2.2500012057142,2.68507411790788));
#11002=CARTESIAN_POINT('Origin',(-14.4886967768384,2.2500012057142,4.11228191177209));
#11003=CARTESIAN_POINT('Origin',(-16.3206772921779,-4.87810968301463,0.853093602568413));
#11004=CARTESIAN_POINT('Origin',(-16.3206772921779,4.87789031698537,0.853093602568413));
#11005=CARTESIAN_POINT('Origin',(-14.4886967768384,2.2500012057142,4.11228191177209));
#11006=CARTESIAN_POINT('Origin',(-17.6706772921778,1.20571420388653E-6,
0.930301396432626));
#11007=CARTESIAN_POINT('Origin',(-17.6706772921778,1.20571420388653E-6,
0.930301396432626));
#11008=CARTESIAN_POINT('Origin',(-16.2434694983136,1.20571420388653E-6,
-0.496906397431586));
#11009=CARTESIAN_POINT('Origin',(-16.2434694983136,1.20571420388653E-6,
-0.496906397431586));
#11010=CARTESIAN_POINT('Origin',(-13.0614889829742,3.97811209444304,2.68507411790788));
#11011=CARTESIAN_POINT('Origin',(-0.0886968229780924,1.20571420388653E-6,
42.7793514595497));
#11012=CARTESIAN_POINT('',(-4.08789728409425,-3.97810968301463,42.7793514595497));
#11013=CARTESIAN_POINT('',(3.91050363813806,-3.97810968301463,42.7793514595497));
#11014=CARTESIAN_POINT('',(6.61050363813806,-3.97810968301463,42.7793514595497));
#11015=CARTESIAN_POINT('',(3.91050363813806,3.97811209444304,42.7793514595497));
#11016=CARTESIAN_POINT('',(3.91050363813806,3.97811209444304,42.7793514595497));
#11017=CARTESIAN_POINT('',(-4.08789728409425,3.97811209444304,42.7793514595497));
#11018=CARTESIAN_POINT('',(6.61050363813806,3.97811209444304,42.7793514595497));
#11019=CARTESIAN_POINT('',(-4.08789728409424,-3.97810968301463,42.7793514595497));
#11020=CARTESIAN_POINT('Origin',(6.61050363813806,-3.97810968301463,-1.39780639743159));
#11021=CARTESIAN_POINT('',(6.61050363813806,-3.97810968301463,40.0793514595497));
#11022=CARTESIAN_POINT('',(6.61050363813806,-3.97810968301463,-1.39780639743159));
#11023=CARTESIAN_POINT('Origin',(3.91050363813806,-3.97810968301463,40.0793514595497));
#11024=CARTESIAN_POINT('',(-6.78789728409425,-3.97810968301463,40.0793514595497));
#11025=CARTESIAN_POINT('Origin',(-4.08789728409424,-3.97810968301463,40.0793514595497));
#11026=CARTESIAN_POINT('',(-6.78789728409425,-3.97810968301463,-1.39780639743159));
#11027=CARTESIAN_POINT('Origin',(6.61050363813806,3.97811209444304,-1.39780639743159));
#11028=CARTESIAN_POINT('',(6.61050363813806,3.97811209444304,40.0793514595497));
#11029=CARTESIAN_POINT('',(6.61050363813806,3.97811209444304,-1.39780639743159));
#11030=CARTESIAN_POINT('',(6.61050363813806,-3.97810968301463,40.0793514595497));
#11031=CARTESIAN_POINT('Origin',(6.61050363813806,3.97811209444304,-1.39780639743159));
#11032=CARTESIAN_POINT('Origin',(3.91050363813806,3.97811209444304,40.0793514595497));
#11033=CARTESIAN_POINT('',(-6.78789728409425,3.97811209444304,40.0793514595497));
#11034=CARTESIAN_POINT('',(-6.78789728409425,3.97811209444304,-1.39780639743159));
#11035=CARTESIAN_POINT('Origin',(-4.08789728409424,3.97811209444304,40.0793514595497));
#11036=CARTESIAN_POINT('Origin',(-6.78789728409425,3.97811209444304,-1.39780639743159));
#11037=CARTESIAN_POINT('',(-6.78789728409425,3.97811209444304,40.0793514595497));
#11038=CARTESIAN_POINT('Origin',(3.91050363813806,1.20571420388653E-6,40.0793514595497));
#11039=CARTESIAN_POINT('Origin',(-4.08789728409424,1.20571420388653E-6,
40.0793514595497));
#11040=CARTESIAN_POINT('Origin',(15.9282673556341,20.,0.0390576814896602));
#11041=CARTESIAN_POINT('',(3.79009320173104,20.,9.63818989051917));
#11042=CARTESIAN_POINT('Origin',(15.9282673556341,20.,0.0390576814896602));
#11043=CARTESIAN_POINT('',(3.79009320173104,20.,9.63818989051917));
#11044=CARTESIAN_POINT('Origin',(-4.05358917681673,20.,15.8411445690945));
#11045=CARTESIAN_POINT('Origin',(-4.05358917681673,20.,15.8411445690945));
#11046=CARTESIAN_POINT('Origin',(-0.0886968229780924,1.205714200531E-6,
16.8344044426714));
#11047=CARTESIAN_POINT('',(0.,0.,0.));
#11048=CARTESIAN_POINT('Origin',(-0.178867612462208,4.46390384366945,37.06975632091));
#11049=CARTESIAN_POINT('',(-0.178867612462208,3.53610097918737,38.26975632091));
#11050=CARTESIAN_POINT('Origin',(-0.178867612462208,3.53610097918737,37.06975632091));
#11051=CARTESIAN_POINT('',(-0.178867612462208,-3.53609615633055,38.26975632091));
#11052=CARTESIAN_POINT('',(-0.178867612462208,4.46390384366945,38.26975632091));
#11053=CARTESIAN_POINT('Origin',(-0.178867612462208,-3.53609615633055,37.06975632091));
#11054=CARTESIAN_POINT('Origin',(-14.6061395505208,-4.33609615633055,3.29091815733825));
#11055=CARTESIAN_POINT('',(-14.6061395505208,4.33590384366945,2.49091815733825));
#11056=CARTESIAN_POINT('Origin',(-14.6061395505208,4.33590384366945,3.29091815733825));
#11057=CARTESIAN_POINT('',(-14.6061395505208,3.53610097918737,2.49091815733825));
#11058=CARTESIAN_POINT('',(-14.6061395505208,-4.33609615633055,2.49091815733825));
#11059=CARTESIAN_POINT('Origin',(-14.6061395505208,3.53610097918737,3.29091815733825));
#11060=CARTESIAN_POINT('Origin',(-14.6061395505208,-4.33609615633055,3.29091815733825));
#11061=CARTESIAN_POINT('',(-14.6061395505208,-3.53609615633055,2.49091815733825));
#11062=CARTESIAN_POINT('Origin',(-14.6061395505208,-3.53609615633055,3.29091815733825));
#11063=CARTESIAN_POINT('',(-14.6061395505208,-4.33609615633055,2.49091815733825));
#11064=CARTESIAN_POINT('',(-14.6061395505208,-4.33609615633055,2.49091815733825));
#11065=CARTESIAN_POINT('Origin',(-14.6061395505208,-4.33609615633055,3.29091815733825));
#11066=CARTESIAN_POINT('Origin',(-14.6061395505208,-4.33609615633055,3.29091815733825));
#11067=CARTESIAN_POINT('',(-14.6061395505208,2.00000241142841,2.49091815733825));
#11068=CARTESIAN_POINT('Origin',(-14.6061395505208,2.00000241142841,3.29091815733825));
#11069=CARTESIAN_POINT('',(-14.6061395505208,-1.99999758857159,2.49091815733825));
#11070=CARTESIAN_POINT('',(-14.6061395505208,-4.33609615633055,2.49091815733825));
#11071=CARTESIAN_POINT('Origin',(-14.6061395505208,-1.99999758857159,3.29091815733825));
#11072=CARTESIAN_POINT('Origin',(-0.177712466787677,14.4000024114284,11.6951080862604));
#11073=CARTESIAN_POINT('',(-0.177712466787678,-5.9999975885716,12.8951080862604));
#11074=CARTESIAN_POINT('Origin',(-0.177712466787677,-5.9999975885716,11.6951080862604));
#11075=CARTESIAN_POINT('',(-0.177712466787678,-10.2544850951109,12.8951080862604));
#11076=CARTESIAN_POINT('',(-0.177712466787678,14.4000024114284,12.8951080862604));
#11077=CARTESIAN_POINT('',(-0.177712466787677,-10.2963772509386,10.4951080862604));
#11078=CARTESIAN_POINT('Ctrl Pts',(-0.177712466787677,-10.2544850951109,
12.8951080862604));
#11079=CARTESIAN_POINT('Ctrl Pts',(-0.328316799600617,-10.2544850951109,
12.8951080862604));
#11080=CARTESIAN_POINT('Ctrl Pts',(-0.488902932607147,-10.2513527873625,
12.8650249475386));
#11081=CARTESIAN_POINT('Ctrl Pts',(-0.78426488938881,-10.2402603738984,
12.742790826072));
#11082=CARTESIAN_POINT('Ctrl Pts',(-0.919050045771719,-10.2324873030817,
12.6506454931746));
#11083=CARTESIAN_POINT('Ctrl Pts',(-1.13193181191228,-10.2185593746734,
12.4381249833728));
#11084=CARTESIAN_POINT('Ctrl Pts',(-1.22429085128089,-10.2115028582253,
12.3035493595844));
#11085=CARTESIAN_POINT('Ctrl Pts',(-1.34702914180779,-10.2033604971208,
12.0085177147771));
#11086=CARTESIAN_POINT('Ctrl Pts',(-1.37740318454924,-10.2024688739752,
11.8480541988248));
#11087=CARTESIAN_POINT('Ctrl Pts',(-1.37801799011132,-10.2076973349447,
11.5464521222423));
#11088=CARTESIAN_POINT('Ctrl Pts',(-1.34806997449904,-10.2141906775384,
11.3853937554379));
#11089=CARTESIAN_POINT('Ctrl Pts',(-1.22585140243605,-10.232651025804,11.0892496287149));
#11090=CARTESIAN_POINT('Ctrl Pts',(-1.13359030470793,-10.244422653795,10.9541478187001));
#11091=CARTESIAN_POINT('Ctrl Pts',(-0.920648927729036,-10.2657970316571,
10.7407719255541));
#11092=CARTESIAN_POINT('Ctrl Pts',(-0.785732755478035,-10.2767999672427,
10.6482195366313));
#11093=CARTESIAN_POINT('Ctrl Pts',(-0.489813246463523,-10.2921837256933,
10.5253827273461));
#11094=CARTESIAN_POINT('Ctrl Pts',(-0.328796143270408,-10.2963772509386,
10.4951080862604));
#11095=CARTESIAN_POINT('Ctrl Pts',(-0.177712466787678,-10.2963772509386,
10.4951080862604));
#11096=CARTESIAN_POINT('Ctrl Pts',(-0.177712466787677,-10.2963772509386,
10.4951080862604));
#11097=CARTESIAN_POINT('Ctrl Pts',(-0.0266287903049468,-10.2963772509386,
10.4951080862604));
#11098=CARTESIAN_POINT('Ctrl Pts',(0.134388312888168,-10.2921837256933,
10.5253827273461));
#11099=CARTESIAN_POINT('Ctrl Pts',(0.430307821902681,-10.2767999672427,
10.6482195366313));
#11100=CARTESIAN_POINT('Ctrl Pts',(0.565223994153682,-10.2657970316571,
10.7407719255541));
#11101=CARTESIAN_POINT('Ctrl Pts',(0.778165371132575,-10.244422653795,10.9541478187001));
#11102=CARTESIAN_POINT('Ctrl Pts',(0.870426468860694,-10.232651025804,11.0892496287149));
#11103=CARTESIAN_POINT('Ctrl Pts',(0.992645040923687,-10.2141906775384,
11.3853937554379));
#11104=CARTESIAN_POINT('Ctrl Pts',(1.02259305653596,-10.2076973349447,11.5464521222423));
#11105=CARTESIAN_POINT('Ctrl Pts',(1.02228504001405,-10.2050778850534,11.6975542403122));
#11106=CARTESIAN_POINT('Ctrl Pts',(1.02197825097388,-10.2024688739752,11.8480541988248));
#11107=CARTESIAN_POINT('Ctrl Pts',(0.991604208232437,-10.2033604971208,
12.0085177147771));
#11108=CARTESIAN_POINT('Ctrl Pts',(0.868865917705535,-10.2115028582253,
12.3035493595844));
#11109=CARTESIAN_POINT('Ctrl Pts',(0.776506878336926,-10.2185593746734,
12.4381249833728));
#11110=CARTESIAN_POINT('Ctrl Pts',(0.563625112196363,-10.2324873030817,
12.6506454931746));
#11111=CARTESIAN_POINT('Ctrl Pts',(0.428839955813454,-10.2402603738984,
12.742790826072));
#11112=CARTESIAN_POINT('Ctrl Pts',(0.133477999031791,-10.2513527873625,
12.8650249475386));
#11113=CARTESIAN_POINT('Ctrl Pts',(-0.0271081339747381,-10.2544850951109,
12.8951080862604));
#11114=CARTESIAN_POINT('Ctrl Pts',(-0.177712466787678,-10.2544850951109,
12.8951080862604));
#11115=CARTESIAN_POINT('Origin',(-0.177712466787677,14.4000024114284,11.6951080862604));
#11116=CARTESIAN_POINT('',(-0.177712466787399,10.2963820737958,10.4951080862576));
#11117=CARTESIAN_POINT('',(-0.177712466787677,10.2544899179677,12.8951080862604));
#11118=CARTESIAN_POINT('Ctrl Pts',(-0.177712466787677,10.2963820737954,
10.4951080862604));
#11119=CARTESIAN_POINT('Ctrl Pts',(-0.328796143270408,10.2963820737954,
10.4951080862604));
#11120=CARTESIAN_POINT('Ctrl Pts',(-0.489813246463523,10.2921885485501,
10.5253827273461));
#11121=CARTESIAN_POINT('Ctrl Pts',(-0.785732755478036,10.2768047900996,
10.6482195366313));
#11122=CARTESIAN_POINT('Ctrl Pts',(-0.920648927729037,10.2658018545139,
10.7407719255541));
#11123=CARTESIAN_POINT('Ctrl Pts',(-1.13359030470793,10.2444274766519,10.9541478187001));
#11124=CARTESIAN_POINT('Ctrl Pts',(-1.22585140243605,10.2326558486608,11.0892496287149));
#11125=CARTESIAN_POINT('Ctrl Pts',(-1.34806997449904,10.2141955003952,11.3853937554379));
#11126=CARTESIAN_POINT('Ctrl Pts',(-1.37801799011132,10.2077021578015,11.5464521222423));
#11127=CARTESIAN_POINT('Ctrl Pts',(-1.37740318454924,10.202473696832,11.8480541988248));
#11128=CARTESIAN_POINT('Ctrl Pts',(-1.34702914180779,10.2033653199776,12.0085177147771));
#11129=CARTESIAN_POINT('Ctrl Pts',(-1.22429085128089,10.2115076810821,12.3035493595844));
#11130=CARTESIAN_POINT('Ctrl Pts',(-1.13193181191228,10.2185641975303,12.4381249833728));
#11131=CARTESIAN_POINT('Ctrl Pts',(-0.919050045771718,10.2324921259385,
12.6506454931746));
#11132=CARTESIAN_POINT('Ctrl Pts',(-0.78426488938881,10.2402651967552,12.742790826072));
#11133=CARTESIAN_POINT('Ctrl Pts',(-0.488902932607147,10.2513576102193,
12.8650249475386));
#11134=CARTESIAN_POINT('Ctrl Pts',(-0.328316799600617,10.2544899179677,
12.8951080862604));
#11135=CARTESIAN_POINT('Ctrl Pts',(-0.177712466787677,10.2544899179677,
12.8951080862604));
#11136=CARTESIAN_POINT('',(-0.177712466787678,6.00000241142841,12.8951080862604));
#11137=CARTESIAN_POINT('',(-0.177712466787678,14.4000024114284,12.8951080862604));
#11138=CARTESIAN_POINT('Origin',(-0.177712466787677,6.00000241142841,11.6951080862604));
#11139=CARTESIAN_POINT('Ctrl Pts',(-0.177712466787677,10.2544899179677,
12.8951080862604));
#11140=CARTESIAN_POINT('Ctrl Pts',(-0.0271081339747375,10.2544899179677,
12.8951080862604));
#11141=CARTESIAN_POINT('Ctrl Pts',(0.133477999031794,10.2513576102193,12.8650249475386));
#11142=CARTESIAN_POINT('Ctrl Pts',(0.428839955813457,10.2402651967552,12.742790826072));
#11143=CARTESIAN_POINT('Ctrl Pts',(0.563625112196364,10.2324921259385,12.6506454931746));
#11144=CARTESIAN_POINT('Ctrl Pts',(0.776506878336926,10.2185641975303,12.4381249833728));
#11145=CARTESIAN_POINT('Ctrl Pts',(0.868865917705535,10.2115076810821,12.3035493595844));
#11146=CARTESIAN_POINT('Ctrl Pts',(0.991604208232437,10.2033653199776,12.0085177147771));
#11147=CARTESIAN_POINT('Ctrl Pts',(1.02197825097388,10.202473696832,11.8480541988248));
#11148=CARTESIAN_POINT('Ctrl Pts',(1.02228504001405,10.2050827079102,11.6975542403122));
#11149=CARTESIAN_POINT('Ctrl Pts',(1.02259305653596,10.2077021578015,11.5464521222423));
#11150=CARTESIAN_POINT('Ctrl Pts',(0.992645040923687,10.2141955003952,11.3853937554379));
#11151=CARTESIAN_POINT('Ctrl Pts',(0.870426468860694,10.2326558486608,11.0892496287149));
#11152=CARTESIAN_POINT('Ctrl Pts',(0.778165371132575,10.2444274766519,10.9541478187001));
#11153=CARTESIAN_POINT('Ctrl Pts',(0.565223994153682,10.2658018545139,10.7407719255541));
#11154=CARTESIAN_POINT('Ctrl Pts',(0.43030782190268,10.2768047900996,10.6482195366313));
#11155=CARTESIAN_POINT('Ctrl Pts',(0.134388312888167,10.2921885485501,10.5253827273461));
#11156=CARTESIAN_POINT('Ctrl Pts',(-0.0266287903049473,10.2963820737954,
10.4951080862604));
#11157=CARTESIAN_POINT('Ctrl Pts',(-0.177712466787678,10.2963820737954,
10.4951080862604));
#11158=CARTESIAN_POINT('Origin',(-0.177712466787677,2.4114284077716E-6,
4.5587029190994));
#11159=CARTESIAN_POINT('',(8.03340298017176,-5.9999975885716,17.7536548280821));
#11160=CARTESIAN_POINT('',(8.03340298017176,6.00000241142841,17.7536548280823));
#11161=CARTESIAN_POINT('Origin',(-0.177712466787677,2.41142840473211E-6,
17.7536548280821));
#11162=CARTESIAN_POINT('',(8.07877050835459,6.00000241142841,15.6530982149009));
#11163=CARTESIAN_POINT('Ctrl Pts',(8.07877050835459,6.00000241142841,15.6530982149009));
#11164=CARTESIAN_POINT('Ctrl Pts',(8.06366240243391,6.00000241142841,16.3532840635641));
#11165=CARTESIAN_POINT('Ctrl Pts',(8.04853997260142,6.00000241142841,17.0534696033076));
#11166=CARTESIAN_POINT('Ctrl Pts',(8.03340298017176,6.00000241142841,17.7536548280823));
#11167=CARTESIAN_POINT('',(6.42417721261747,7.81192895720387,14.4149297172206));
#11168=CARTESIAN_POINT('Ctrl Pts',(6.42417721261747,7.81192895720387,14.4149297172206));
#11169=CARTESIAN_POINT('Ctrl Pts',(6.61539136987313,7.64482915707008,14.6557669349746));
#11170=CARTESIAN_POINT('Ctrl Pts',(6.84457822090961,7.43072762012922,14.8799697306037));
#11171=CARTESIAN_POINT('Ctrl Pts',(7.27350466710297,6.99326166671321,15.2278608961883));
#11172=CARTESIAN_POINT('Ctrl Pts',(7.52472544806286,6.71464397987196,15.3881604696605));
#11173=CARTESIAN_POINT('Ctrl Pts',(7.87311364932487,6.27809195147036,15.5649909889583));
#11174=CARTESIAN_POINT('Ctrl Pts',(7.97807672550604,6.13977704927159,15.6122830391166));
#11175=CARTESIAN_POINT('Ctrl Pts',(8.07877050835459,6.0000024114284,15.6530982149009));
#11176=CARTESIAN_POINT('',(4.37105054513769,9.20455838802752,12.1676472976633));
#11177=CARTESIAN_POINT('Ctrl Pts',(6.42417721261747,7.81192895720387,14.4149297172206));
#11178=CARTESIAN_POINT('Ctrl Pts',(5.80201464762526,8.35562949566307,13.6313062486766));
#11179=CARTESIAN_POINT('Ctrl Pts',(5.1062543034617,8.82759075958201,12.8682159131197));
#11180=CARTESIAN_POINT('Ctrl Pts',(4.37105054513769,9.20455838802752,12.1676472976633));
#11181=CARTESIAN_POINT('',(3.31160798786662,9.67660434821715,11.0613919569551));
#11182=CARTESIAN_POINT('Ctrl Pts',(3.31160798786662,9.67660434821715,11.0613919569551));
#11183=CARTESIAN_POINT('Ctrl Pts',(3.38725054660564,9.64772154529681,11.1479758305217));
#11184=CARTESIAN_POINT('Ctrl Pts',(3.46338662895692,9.61766757102202,11.2333252889551));
#11185=CARTESIAN_POINT('Ctrl Pts',(3.80017953593501,9.48013167695816,11.6032638240621));
#11186=CARTESIAN_POINT('Ctrl Pts',(4.08032391034575,9.35362526751858,11.8906166735587));
#11187=CARTESIAN_POINT('Ctrl Pts',(4.37105054513769,9.20455838802752,12.1676472976633));
#11188=CARTESIAN_POINT('',(-2.13351287620983,10.1557585661665,7.86054193760863));
#11189=CARTESIAN_POINT('Ctrl Pts',(3.31160798786662,9.67660434821715,11.0613919569551));
#11190=CARTESIAN_POINT('Ctrl Pts',(3.30666333464517,9.67849237853878,11.0557320845698));
#11191=CARTESIAN_POINT('Ctrl Pts',(3.3017142876189,9.68037750652116,11.0500800606398));
#11192=CARTESIAN_POINT('Ctrl Pts',(2.92188570807458,9.82470497845806,10.617283747585));
#11193=CARTESIAN_POINT('Ctrl Pts',(2.47116292610906,9.96831796451907,10.1818454164884));
#11194=CARTESIAN_POINT('Ctrl Pts',(1.4848560953238,10.1931375646734,9.40301401138184));
#11195=CARTESIAN_POINT('Ctrl Pts',(0.94889137476814,10.2728830446272,9.05968197552145));
#11196=CARTESIAN_POINT('Ctrl Pts',(-0.343612808630755,10.3610965901736,
8.38073343101154));
#11197=CARTESIAN_POINT('Ctrl Pts',(-1.23584670217506,10.3252285394421,8.051982603611));
#11198=CARTESIAN_POINT('Ctrl Pts',(-2.13351287620984,10.1557585661665,7.86054193760862));
#11199=CARTESIAN_POINT('',(-9.95140751249447,3.53610017282902,4.91934709248468));
#11200=CARTESIAN_POINT('Ctrl Pts',(-9.95140751249447,3.53610017282902,4.91934709248468));
#11201=CARTESIAN_POINT('Ctrl Pts',(-9.89707498092324,3.68471646024097,4.94970641657277));
#11202=CARTESIAN_POINT('Ctrl Pts',(-9.83935880934888,3.8319721919242,4.98171908114857));
#11203=CARTESIAN_POINT('Ctrl Pts',(-9.24965882931434,5.24053783544831,5.30577915095143));
#11204=CARTESIAN_POINT('Ctrl Pts',(-8.46376367800013,6.37827852692683,5.71189719320963));
#11205=CARTESIAN_POINT('Ctrl Pts',(-6.65732758822298,8.19454584161434,6.50688309595488));
#11206=CARTESIAN_POINT('Ctrl Pts',(-5.49960232856536,8.99469099268257,6.9534533168386));
#11207=CARTESIAN_POINT('Ctrl Pts',(-3.54725844985039,9.81102690694312,7.52942979311924));
#11208=CARTESIAN_POINT('Ctrl Pts',(-2.84446760524541,10.0215377584598,7.70892026491894));
#11209=CARTESIAN_POINT('Ctrl Pts',(-2.13351287620983,10.1557585661665,7.86054193760862));
#11210=CARTESIAN_POINT('',(-9.86226050887947,3.53610097918737,9.71934528208445));
#11211=CARTESIAN_POINT('Ctrl Pts',(-9.95140898508777,3.53610097918737,4.91934626964542));
#11212=CARTESIAN_POINT('Ctrl Pts',(-9.93632582125981,3.53610097918737,5.73181939317775));
#11213=CARTESIAN_POINT('Ctrl Pts',(-9.92124034862481,3.53610097918737,6.54429346176475));
#11214=CARTESIAN_POINT('Ctrl Pts',(-9.90615078043081,3.53610097918737,7.35676745427743));
#11215=CARTESIAN_POINT('Ctrl Pts',(-9.89152455533496,3.53610097918737,8.14429346868886));
#11216=CARTESIAN_POINT('Ctrl Pts',(-9.87689448233653,3.53610097918737,8.93181941162615));
#11217=CARTESIAN_POINT('Ctrl Pts',(-9.86226050887948,3.53610097918737,9.71934528208445));
#11218=CARTESIAN_POINT('',(-10.4876331192705,2.4114284090342E-6,9.71934528208445));
#11219=CARTESIAN_POINT('Origin',(-0.177712466787677,2.4114284077716E-6,
9.71934528208445));
#11220=CARTESIAN_POINT('',(-10.1203897656684,2.41142840880554E-6,30.7587029190994));
#11221=CARTESIAN_POINT('',(-10.5777124667877,2.41142840904524E-6,4.5587029190994));
#11222=CARTESIAN_POINT('',(9.76497550923372,2.41142840604871E-6,30.7580912261184));
#11223=CARTESIAN_POINT('Ctrl Pts',(-10.1203897656684,2.41142840862185E-6,
30.7587029190994));
#11224=CARTESIAN_POINT('Ctrl Pts',(-10.1203897656684,1.27089668043473,30.7587029190994));
#11225=CARTESIAN_POINT('Ctrl Pts',(-9.86008094032418,2.6077169391002,30.9068158434723));
#11226=CARTESIAN_POINT('Ctrl Pts',(-8.83558352698103,5.04135256634328,31.4099925598972));
#11227=CARTESIAN_POINT('Ctrl Pts',(-8.07213111882965,6.14055961719644,31.7549337629918));
#11228=CARTESIAN_POINT('Ctrl Pts',(-6.32709993360833,7.87313335557606,32.3805754170083));
#11229=CARTESIAN_POINT('Ctrl Pts',(-5.22311287806905,8.62972184841935,32.7057628801753));
#11230=CARTESIAN_POINT('Ctrl Pts',(-2.78235121183544,9.64293330397286,33.1623258591164));
#11231=CARTESIAN_POINT('Ctrl Pts',(-1.44421313614939,9.89851844327917,33.2887002128102));
#11232=CARTESIAN_POINT('Ctrl Pts',(1.08880241943988,9.8985196265464,33.2886324234761));
#11233=CARTESIAN_POINT('Ctrl Pts',(2.4269477644944,9.64293055183899,33.1621838232405));
#11234=CARTESIAN_POINT('Ctrl Pts',(4.86771468168172,8.62971246476211,32.7054793231542));
#11235=CARTESIAN_POINT('Ctrl Pts',(5.97170006728986,7.87312153584118,32.3802243211076));
#11236=CARTESIAN_POINT('Ctrl Pts',(7.71672174055816,6.14055081828832,31.7544717166664));
#11237=CARTESIAN_POINT('Ctrl Pts',(8.48016993081502,5.04134981420114,31.409478412752));
#11238=CARTESIAN_POINT('Ctrl Pts',(9.50466493926388,2.60772113563203,30.9062263543421));
#11239=CARTESIAN_POINT('Ctrl Pts',(9.76497550923372,1.27090121854302,30.7580912261184));
#11240=CARTESIAN_POINT('Ctrl Pts',(9.76497550923372,2.41142840889941E-6,
30.7580912261184));
#11241=CARTESIAN_POINT('Ctrl Pts',(9.76497550923372,2.41142840751163E-6,
30.7580912261184));
#11242=CARTESIAN_POINT('Ctrl Pts',(9.76497550923372,-1.2708963956862,30.7580912261184));
#11243=CARTESIAN_POINT('Ctrl Pts',(9.50466493926388,-2.60771631277522,30.9062263543421));
#11244=CARTESIAN_POINT('Ctrl Pts',(8.48016993081501,-5.04134499134433,31.409478412752));
#11245=CARTESIAN_POINT('Ctrl Pts',(7.71672174055816,-6.14054599543151,31.7544717166664));
#11246=CARTESIAN_POINT('Ctrl Pts',(5.97170006728986,-7.87311671298437,32.3802243211076));
#11247=CARTESIAN_POINT('Ctrl Pts',(4.86771468168172,-8.62970764190529,32.7054793231542));
#11248=CARTESIAN_POINT('Ctrl Pts',(2.4269477644944,-9.64292572898218,33.1621838232405));
#11249=CARTESIAN_POINT('Ctrl Pts',(1.08880241943988,-9.89851480368958,33.2886324234761));
#11250=CARTESIAN_POINT('Ctrl Pts',(-1.44421313614939,-9.89851362042235,
33.2887002128102));
#11251=CARTESIAN_POINT('Ctrl Pts',(-2.78235121183544,-9.64292848111604,
33.1623258591164));
#11252=CARTESIAN_POINT('Ctrl Pts',(-5.22311287806905,-8.62971702556254,
32.7057628801753));
#11253=CARTESIAN_POINT('Ctrl Pts',(-6.32709993360833,-7.87312853271924,
32.3805754170083));
#11254=CARTESIAN_POINT('Ctrl Pts',(-8.07213111882965,-6.14055479433963,
31.7549337629918));
#11255=CARTESIAN_POINT('Ctrl Pts',(-8.83558352698103,-5.04134774348647,
31.4099925598972));
#11256=CARTESIAN_POINT('Ctrl Pts',(-9.86008094032418,-2.60771211624338,
30.9068158434723));
#11257=CARTESIAN_POINT('Ctrl Pts',(-10.1203897656684,-1.27089185757792,
30.7587029190994));
#11258=CARTESIAN_POINT('Ctrl Pts',(-10.1203897656684,2.41142840695652E-6,
30.7587029190994));
#11259=CARTESIAN_POINT('',(-9.86226050887947,-3.53609615633055,9.71934528208445));
#11260=CARTESIAN_POINT('Origin',(-0.177712466787677,2.4114284077716E-6,
9.71934528208445));
#11261=CARTESIAN_POINT('',(-9.95140789577959,-3.53609567260447,4.91934619906695));
#11262=CARTESIAN_POINT('Ctrl Pts',(-9.86226050887948,-3.53609615633055,
9.71934528208445));
#11263=CARTESIAN_POINT('Ctrl Pts',(-9.87689448233653,-3.53609615633055,
8.93181941162615));
#11264=CARTESIAN_POINT('Ctrl Pts',(-9.89152455533695,-3.53609615633055,
8.14429346867934));
#11265=CARTESIAN_POINT('Ctrl Pts',(-9.90615078043284,-3.53609615633055,
7.35676745426777));
#11266=CARTESIAN_POINT('Ctrl Pts',(-9.92124034862687,-3.53609615633055,
6.54429346175493));
#11267=CARTESIAN_POINT('Ctrl Pts',(-9.93632582125982,-3.53609615633055,
5.73181939317775));
#11268=CARTESIAN_POINT('Ctrl Pts',(-9.95140898508777,-3.53609615633055,
4.91934626964541));
#11269=CARTESIAN_POINT('',(-2.13351287620984,-10.1557537433096,7.86054193760862));
#11270=CARTESIAN_POINT('Ctrl Pts',(-2.13351287620984,-10.1557537433096,
7.86054193760862));
#11271=CARTESIAN_POINT('Ctrl Pts',(-2.84446760524542,-10.021532935603,7.70892026491893));
#11272=CARTESIAN_POINT('Ctrl Pts',(-3.54725844985039,-9.8110220840863,7.52942979311924));
#11273=CARTESIAN_POINT('Ctrl Pts',(-5.49960232856536,-8.99468616982575,
6.9534533168386));
#11274=CARTESIAN_POINT('Ctrl Pts',(-6.65732758822298,-8.19454101875751,
6.50688309595488));
#11275=CARTESIAN_POINT('Ctrl Pts',(-8.46376367800012,-6.37827370407001,
5.71189719320963));
#11276=CARTESIAN_POINT('Ctrl Pts',(-9.24965882931434,-5.2405330125915,5.30577915095143));
#11277=CARTESIAN_POINT('Ctrl Pts',(-9.83935880934888,-3.83196736906738,
4.98171908114857));
#11278=CARTESIAN_POINT('Ctrl Pts',(-9.89707498092324,-3.68471163738415,
4.94970641657277));
#11279=CARTESIAN_POINT('Ctrl Pts',(-9.95140751249447,-3.5360953499722,4.91934709248468));
#11280=CARTESIAN_POINT('',(3.31160798786661,-9.67659952536034,11.0613919569551));
#11281=CARTESIAN_POINT('Ctrl Pts',(-2.13351287620984,-10.1557537433096,
7.86054193760862));
#11282=CARTESIAN_POINT('Ctrl Pts',(-1.23584670217506,-10.3252237165853,
8.051982603611));
#11283=CARTESIAN_POINT('Ctrl Pts',(-0.343612808630755,-10.3610917673168,
8.38073343101154));
#11284=CARTESIAN_POINT('Ctrl Pts',(0.948891374768143,-10.2728782217704,
9.05968197552145));
#11285=CARTESIAN_POINT('Ctrl Pts',(1.48485609532381,-10.1931327418166,9.40301401138184));
#11286=CARTESIAN_POINT('Ctrl Pts',(2.47116292610906,-9.96831314166225,10.1818454164884));
#11287=CARTESIAN_POINT('Ctrl Pts',(2.92188570807458,-9.82470015560125,10.617283747585));
#11288=CARTESIAN_POINT('Ctrl Pts',(3.3017142876189,-9.68037268366434,11.0500800606398));
#11289=CARTESIAN_POINT('Ctrl Pts',(3.30666333464517,-9.67848755568196,11.0557320845698));
#11290=CARTESIAN_POINT('Ctrl Pts',(3.31160798786662,-9.67659952536034,11.0613919569551));
#11291=CARTESIAN_POINT('',(4.37105054513769,-9.2045535651707,12.1676472976633));
#11292=CARTESIAN_POINT('Ctrl Pts',(4.37105054513769,-9.2045535651707,12.1676472976633));
#11293=CARTESIAN_POINT('Ctrl Pts',(4.08032391034576,-9.35362044466177,11.8906166735587));
#11294=CARTESIAN_POINT('Ctrl Pts',(3.80017953593501,-9.48012685410135,11.6032638240621));
#11295=CARTESIAN_POINT('Ctrl Pts',(3.46338662895692,-9.6176627481652,11.2333252889551));
#11296=CARTESIAN_POINT('Ctrl Pts',(3.38725054660564,-9.64771672243999,11.1479758305217));
#11297=CARTESIAN_POINT('Ctrl Pts',(3.31160798786662,-9.67659952536034,11.0613919569551));
#11298=CARTESIAN_POINT('',(6.42417721261744,-7.81192413434708,14.4149297172206));
#11299=CARTESIAN_POINT('Ctrl Pts',(4.37105054513769,-9.2045535651707,12.1676472976633));
#11300=CARTESIAN_POINT('Ctrl Pts',(5.10619880095024,-8.82761439502656,12.8681630253085));
#11301=CARTESIAN_POINT('Ctrl Pts',(5.80196171161444,-8.3556709329627,13.6312395749441));
#11302=CARTESIAN_POINT('Ctrl Pts',(6.42417721261744,-7.81192413434708,14.4149297172206));
#11303=CARTESIAN_POINT('',(8.07877050835458,-5.9999975885716,15.6530982149009));
#11304=CARTESIAN_POINT('Ctrl Pts',(8.07877050835458,-5.9999975885716,15.6530982149009));
#11305=CARTESIAN_POINT('Ctrl Pts',(7.97807672550604,-6.13977222641478,15.6122830391166));
#11306=CARTESIAN_POINT('Ctrl Pts',(7.87311364932487,-6.27808712861355,15.5649909889583));
#11307=CARTESIAN_POINT('Ctrl Pts',(7.52472544806286,-6.71463915701515,15.3881604696605));
#11308=CARTESIAN_POINT('Ctrl Pts',(7.27350466710297,-6.9932568438564,15.2278608961883));
#11309=CARTESIAN_POINT('Ctrl Pts',(6.8445782209096,-7.43072279727242,14.8799697306037));
#11310=CARTESIAN_POINT('Ctrl Pts',(6.6153913698731,-7.64482433421329,14.6557669349745));
#11311=CARTESIAN_POINT('Ctrl Pts',(6.42417721261744,-7.81192413434708,14.4149297172206));
#11312=CARTESIAN_POINT('Ctrl Pts',(8.03340298017176,-5.9999975885716,17.7536548280821));
#11313=CARTESIAN_POINT('Ctrl Pts',(8.04853997260142,-5.9999975885716,17.0534696033075));
#11314=CARTESIAN_POINT('Ctrl Pts',(8.0636624024339,-5.9999975885716,16.353284063564));
#11315=CARTESIAN_POINT('Ctrl Pts',(8.07877050835458,-5.9999975885716,15.6530982149009));
#11316=CARTESIAN_POINT('Origin',(15.9282673556341,20.,0.0390576814896602));
#11317=CARTESIAN_POINT('',(4.37105054513769,6.00000241142841,12.1676472976633));
#11318=CARTESIAN_POINT('',(4.37105054513769,20.,12.1676472976633));
#11319=CARTESIAN_POINT('',(3.31160798786661,6.00000241142841,11.0613919569551));
#11320=CARTESIAN_POINT('Origin',(15.9282673556341,6.00000241142841,0.0390576814896602));
#11321=CARTESIAN_POINT('',(3.31160798786661,20.,11.0613919569551));
#11322=CARTESIAN_POINT('Origin',(15.9282673556341,20.,0.0390576814896602));
#11323=CARTESIAN_POINT('',(4.37105054513769,-5.99999758857159,12.1676472976633));
#11324=CARTESIAN_POINT('',(3.31160798786661,-5.99999758857159,11.0613919569551));
#11325=CARTESIAN_POINT('Origin',(15.9282673556341,-5.99999758857159,0.0390576814896602));
#11326=CARTESIAN_POINT('',(4.37105054513769,20.,12.1676472976633));
#11327=CARTESIAN_POINT('',(3.31160798786661,20.,11.0613919569551));
#11328=CARTESIAN_POINT('Origin',(-0.177712466787677,2.41142840473615E-6,
17.7187500152076));
#11329=CARTESIAN_POINT('',(5.36743577950585,6.00000241142841,15.7187500152076));
#11330=CARTESIAN_POINT('',(5.36743577950585,-5.9999975885716,15.7187500152076));
#11331=CARTESIAN_POINT('Origin',(-0.177712466787677,2.41142840496745E-6,
15.7187500152076));
#11332=CARTESIAN_POINT('Ctrl Pts',(8.03340298017176,6.00000241142841,17.7536548280823));
#11333=CARTESIAN_POINT('Ctrl Pts',(8.0336564955911,6.00000241142841,17.7419280764372));
#11334=CARTESIAN_POINT('Ctrl Pts',(8.03378024422029,6.00000241142841,17.7302885973412));
#11335=CARTESIAN_POINT('Ctrl Pts',(8.03378024422029,6.00000241142841,17.7187500152076));
#11336=CARTESIAN_POINT('Ctrl Pts',(8.03378024422029,6.00000241142841,17.4922929238556));
#11337=CARTESIAN_POINT('Ctrl Pts',(7.97327314315844,6.00000241142841,17.2273662487111));
#11338=CARTESIAN_POINT('Ctrl Pts',(7.77162808002468,6.00000241142841,16.7923068382797));
#11339=CARTESIAN_POINT('Ctrl Pts',(7.58483347292422,6.00000241142841,16.552880331799));
#11340=CARTESIAN_POINT('Ctrl Pts',(7.16867991474912,6.00000241142841,16.187909747159));
#11341=CARTESIAN_POINT('Ctrl Pts',(6.85309265217151,6.00000241142841,16.0135423105674));
#11342=CARTESIAN_POINT('Ctrl Pts',(6.20801832838943,6.00000241142841,15.7841079557633));
#11343=CARTESIAN_POINT('Ctrl Pts',(5.75163519004221,6.00000241142841,15.7187500152076));
#11344=CARTESIAN_POINT('Ctrl Pts',(5.36743577950585,6.00000241142841,15.7187500152076));
#11345=CARTESIAN_POINT('Ctrl Pts',(5.36743577950585,-5.9999975885716,15.7187500152076));
#11346=CARTESIAN_POINT('Ctrl Pts',(5.72647842293398,-5.9999975885716,15.7187500152076));
#11347=CARTESIAN_POINT('Ctrl Pts',(6.15352297661853,-5.9999975885716,15.7758961583859));
#11348=CARTESIAN_POINT('Ctrl Pts',(6.76579277314527,-5.9999975885716,15.9756283261255));
#11349=CARTESIAN_POINT('Ctrl Pts',(7.07130289664905,-5.9999975885716,16.1292918308475));
#11350=CARTESIAN_POINT('Ctrl Pts',(7.51408278212533,-5.9999975885716,16.4745709963669));
#11351=CARTESIAN_POINT('Ctrl Pts',(7.73059566582944,-5.9999975885716,16.7260080521206));
#11352=CARTESIAN_POINT('Ctrl Pts',(7.96379246621659,-5.9999975885716,17.1910498696455));
#11353=CARTESIAN_POINT('Ctrl Pts',(8.03378024422029,-5.9999975885716,17.4750238564616));
#11354=CARTESIAN_POINT('Ctrl Pts',(8.03378024422029,-5.9999975885716,17.7187500152076));
#11355=CARTESIAN_POINT('Ctrl Pts',(8.03378024422029,-5.9999975885716,17.7302885973412));
#11356=CARTESIAN_POINT('Ctrl Pts',(8.03365649559111,-5.9999975885716,17.741928076437));
#11357=CARTESIAN_POINT('Ctrl Pts',(8.03340298017176,-5.9999975885716,17.7536548280821));
#11358=CARTESIAN_POINT('',(8.34339394095876,2.41142818149586E-6,15.7498126454214));
#11359=CARTESIAN_POINT('Ctrl Pts',(8.70260319627842,2.41142840359115E-6,
15.8491426817344));
#11360=CARTESIAN_POINT('Ctrl Pts',(8.70260319627842,0.1457045944121,15.8491426817344));
#11361=CARTESIAN_POINT('Ctrl Pts',(8.69364580031477,0.296936499486973,15.8471441058903));
#11362=CARTESIAN_POINT('Ctrl Pts',(8.65874844698062,0.550908277238344,15.8389323814439));
#11363=CARTESIAN_POINT('Ctrl Pts',(8.63853053418753,0.646402965673418,15.8340793094607));
#11364=CARTESIAN_POINT('Ctrl Pts',(8.60408557717993,0.759711181045861,15.8254316219397));
#11365=CARTESIAN_POINT('Ctrl Pts',(8.5850108075902,0.815595445147395,15.8206049324342));
#11366=CARTESIAN_POINT('Ctrl Pts',(8.55163815579824,0.871468558310266,15.8117236803648));
#11367=CARTESIAN_POINT('Ctrl Pts',(8.54152593085035,0.885874415477635,15.8090050962758));
#11368=CARTESIAN_POINT('Ctrl Pts',(8.52435773636745,0.901956274035506,15.8042960825429));
#11369=CARTESIAN_POINT('Ctrl Pts',(8.51797517577937,0.906754467657781,15.8025322161507));
#11370=CARTESIAN_POINT('Ctrl Pts',(8.50624686619019,0.912133938580912,15.7992540736978));
#11371=CARTESIAN_POINT('Ctrl Pts',(8.50122322934824,0.91355243852032,15.7978404300894));
#11372=CARTESIAN_POINT('Ctrl Pts',(8.49091881899635,0.91416086088759,15.7949175385542));
#11373=CARTESIAN_POINT('Ctrl Pts',(8.48596709871937,0.913383948477207,15.7935022066964));
#11374=CARTESIAN_POINT('Ctrl Pts',(8.474893845048,0.909319390924804,15.7903156787572));
#11375=CARTESIAN_POINT('Ctrl Pts',(8.46924834293951,0.905476072857559,15.7886748573832));
#11376=CARTESIAN_POINT('Ctrl Pts',(8.45591203444658,0.893350354530391,15.7847743670347));
#11377=CARTESIAN_POINT('Ctrl Pts',(8.44886017802113,0.883355752885808,15.7826834861937));
#11378=CARTESIAN_POINT('Ctrl Pts',(8.42921811137653,0.849625584159388,15.7768229351228));
#11379=CARTESIAN_POINT('Ctrl Pts',(8.41857418536194,0.818832096261853,15.77357085887));
#11380=CARTESIAN_POINT('Ctrl Pts',(8.38963278923615,0.718049400748019,15.7646736905908));
#11381=CARTESIAN_POINT('Ctrl Pts',(8.37640202783079,0.623503318149914,15.7604475541772));
#11382=CARTESIAN_POINT('Ctrl Pts',(8.35677624531277,0.44067682070463,15.7541764262857));
#11383=CARTESIAN_POINT('Ctrl Pts',(8.35027668860286,0.325088164238925,15.7520555912301));
#11384=CARTESIAN_POINT('Ctrl Pts',(8.34306653761666,0.101377390155308,15.7497077216999));
#11385=CARTESIAN_POINT('Ctrl Pts',(8.34243149243459,-0.0207353219056583,
15.7494989245869));
#11386=CARTESIAN_POINT('Ctrl Pts',(8.34693351311756,-0.248426106820748,
15.7509676266811));
#11387=CARTESIAN_POINT('Ctrl Pts',(8.35201202114988,-0.366559655312288,
15.7526295432987));
#11388=CARTESIAN_POINT('Ctrl Pts',(8.3687589044063,-0.562240685563907,15.7580128828001));
#11389=CARTESIAN_POINT('Ctrl Pts',(8.38041238916994,-0.663093948738599,
15.7617584461812));
#11390=CARTESIAN_POINT('Ctrl Pts',(8.40759738858707,-0.783137084891655,
15.7702044457537));
#11391=CARTESIAN_POINT('Ctrl Pts',(8.41958541271743,-0.826709692526858,
15.7739090533259));
#11392=CARTESIAN_POINT('Ctrl Pts',(8.44203546065897,-0.87243390895032,15.7806521090902));
#11393=CARTESIAN_POINT('Ctrl Pts',(8.44958624407923,-0.885261390162398,
15.782905772264));
#11394=CARTESIAN_POINT('Ctrl Pts',(8.46336792824719,-0.900507134123406,
15.7869579908969));
#11395=CARTESIAN_POINT('Ctrl Pts',(8.46876320763649,-0.905270445033883,
15.788535226918));
#11396=CARTESIAN_POINT('Ctrl Pts',(8.47924099692529,-0.911158565852659,
15.7915688525739));
#11397=CARTESIAN_POINT('Ctrl Pts',(8.48394623004557,-0.912880662985735,
15.792923034465));
#11398=CARTESIAN_POINT('Ctrl Pts',(8.49406517207035,-0.914291240571678,
15.7958131414122));
#11399=CARTESIAN_POINT('Ctrl Pts',(8.49915094354501,-0.913869835331626,
15.7972547181197));
#11400=CARTESIAN_POINT('Ctrl Pts',(8.51110380005296,-0.91053442442188,15.800618271558));
#11401=CARTESIAN_POINT('Ctrl Pts',(8.51754939660892,-0.906818762271611,
15.8024119432661));
#11402=CARTESIAN_POINT('Ctrl Pts',(8.53354825296255,-0.894484934836979,
15.806829539192));
#11403=CARTESIAN_POINT('Ctrl Pts',(8.54261523602715,-0.883575448092069,
15.8092896800772));
#11404=CARTESIAN_POINT('Ctrl Pts',(8.57970306582927,-0.830473956918792,
15.8192582016274));
#11405=CARTESIAN_POINT('Ctrl Pts',(8.60192499259373,-0.766124180642222,
15.8248840078164));
#11406=CARTESIAN_POINT('Ctrl Pts',(8.63698938385199,-0.65269060197119,15.8337015828562));
#11407=CARTESIAN_POINT('Ctrl Pts',(8.65729303891214,-0.558598640774244,
15.8385845860059));
#11408=CARTESIAN_POINT('Ctrl Pts',(8.69327905844745,-0.303189203914345,
15.8470644051406));
#11409=CARTESIAN_POINT('Ctrl Pts',(8.70260319627842,-0.148645966954802,
15.8491426817344));
#11410=CARTESIAN_POINT('Ctrl Pts',(8.70260319627842,2.41142840350442E-6,
15.8491426817344));
#11411=CARTESIAN_POINT('Origin',(3.70657129686984,28.8000024114284,-19.5236399353513));
#11412=CARTESIAN_POINT('',(-6.57771246678768,-5.99999758857159,6.51927671137959));
#11413=CARTESIAN_POINT('',(-2.13351287620984,-5.9999975885716,7.86054193760862));
#11414=CARTESIAN_POINT('Origin',(3.70657129686984,-5.99999758857159,-19.5236399353513));
#11415=CARTESIAN_POINT('',(-2.13351287620984,28.8000024114284,7.86054193760862));
#11416=CARTESIAN_POINT('Ctrl Pts',(-9.95140751249447,-3.53609534997221,
4.91934709248468));
#11417=CARTESIAN_POINT('Ctrl Pts',(-10.368177467718,-2.39610055019092,4.68646903996433));
#11418=CARTESIAN_POINT('Ctrl Pts',(-10.5777124667877,-1.17144708556741,
4.5587029190994));
#11419=CARTESIAN_POINT('Ctrl Pts',(-10.5777124667877,1.17145190842423,4.5587029190994));
#11420=CARTESIAN_POINT('Ctrl Pts',(-10.368177467718,2.39610537304773,4.68646903996433));
#11421=CARTESIAN_POINT('Ctrl Pts',(-9.95140751249447,3.53610017282902,4.91934709248468));
#11422=CARTESIAN_POINT('',(-2.13351287620984,6.00000241142841,7.86054193760862));
#11423=CARTESIAN_POINT('',(-2.13351287620984,28.8000024114284,7.86054193760862));
#11424=CARTESIAN_POINT('',(-6.57771246678768,6.00000241142841,6.51927671137958));
#11425=CARTESIAN_POINT('Origin',(3.70657129686984,6.00000241142841,-19.5236399353513));
#11426=CARTESIAN_POINT('',(-6.57771246678768,28.8000024114284,6.51927671137959));
#11427=CARTESIAN_POINT('Origin',(-9.15718923943328,2.4114284077716E-6,-4.42077385354621));
#11428=CARTESIAN_POINT('',(-15.1031958253685,-3.53609615633055,1.52523273238902));
#11429=CARTESIAN_POINT('',(-16.37182497547,-3.53609615633055,2.79386188249054));
#11430=CARTESIAN_POINT('',(-14.5375104004193,-3.53609615633055,0.959547307439778));
#11431=CARTESIAN_POINT('',(-16.37182497547,-1.99999758857159,2.79386188249054));
#11432=CARTESIAN_POINT('',(-16.37182497547,-1.99999758857159,2.79386188249054));
#11433=CARTESIAN_POINT('',(-15.1031958253685,-1.99999758857159,1.52523273238902));
#11434=CARTESIAN_POINT('',(-9.15718923943328,-1.99999758857159,-4.42077385354621));
#11435=CARTESIAN_POINT('',(-15.1031958253685,-3.53609615633055,1.52523273238902));
#11436=CARTESIAN_POINT('Origin',(-0.177712466787677,2.4114284077716E-6,
4.5587029190994));
#11437=CARTESIAN_POINT('Origin',(-0.177712466787677,2.4114284077716E-6,
4.91934528208444));
#11438=CARTESIAN_POINT('Origin',(-0.17826912272476,28.8000024114284,12.4886663257821));
#11439=CARTESIAN_POINT('',(5.77713238753779,-3.53609615633055,32.417870847076));
#11440=CARTESIAN_POINT('',(5.77713238753779,3.53610097918737,32.417870847076));
#11441=CARTESIAN_POINT('',(5.77713238753779,28.8000024114284,32.417870847076));
#11442=CARTESIAN_POINT('',(-6.13255732111315,-3.53609615633055,32.4182035018063));
#11443=CARTESIAN_POINT('Origin',(-0.17826912272476,-3.53609615633055,12.4886663257821));
#11444=CARTESIAN_POINT('',(-6.13255732111315,3.53610097918737,32.4182035018063));
#11445=CARTESIAN_POINT('',(-6.13255732111315,28.8000024114284,32.4182035018063));
#11446=CARTESIAN_POINT('Origin',(-0.17826912272476,3.53610097918737,12.4886663257821));
#11447=CARTESIAN_POINT('Origin',(12.6222875332123,6.00000241142841,15.7187500152076));
#11448=CARTESIAN_POINT('',(-6.57771246678768,-5.9999975885716,15.7187500152076));
#11449=CARTESIAN_POINT('',(12.6222875332123,-5.9999975885716,15.7187500152076));
#11450=CARTESIAN_POINT('',(-6.57771246678768,6.00000241142841,15.7187500152076));
#11451=CARTESIAN_POINT('',(-6.57771246678768,6.00000241142841,15.7187500152076));
#11452=CARTESIAN_POINT('',(12.6222875332123,6.00000241142841,15.7187500152076));
#11453=CARTESIAN_POINT('Origin',(12.6222875332123,-5.99999758857159,-6.60134417700877));
#11454=CARTESIAN_POINT('',(6.42417721261744,-5.9999975885716,14.4149297172206));
#11455=CARTESIAN_POINT('Origin',(9.60397861284329,-5.9999975885716,11.8903072744979));
#11456=CARTESIAN_POINT('Origin',(-10.8056176096432,-5.9999975885716,28.0946289238114));
#11457=CARTESIAN_POINT('Origin',(-4.21925722373829,-5.9999975885716,17.6406068922372));
#11458=CARTESIAN_POINT('',(-6.57771246678768,-5.99999758857159,-6.60134417700877));
#11459=CARTESIAN_POINT('Origin',(12.6222875332123,6.00000241142841,-6.60134417700877));
#11460=CARTESIAN_POINT('',(6.42417721261744,6.00000241142841,14.4149297172206));
#11461=CARTESIAN_POINT('Origin',(-10.8056176096432,6.0000024114284,28.0946289238114));
#11462=CARTESIAN_POINT('Origin',(9.60397861284329,6.00000241142841,11.8903072744979));
#11463=CARTESIAN_POINT('',(-6.57771246678768,6.00000241142841,-6.60134417700877));
#11464=CARTESIAN_POINT('Origin',(-4.21925722373829,6.0000024114284,17.6406068922372));
#11465=CARTESIAN_POINT('Origin',(-6.57771246678768,2.4114284077716E-6,4.5587029190994));
#11466=CARTESIAN_POINT('Origin',(10.4270144578429,-3.53609615633055,4.91934528208444));
#11467=CARTESIAN_POINT('',(-10.5777124257746,-3.53609615633055,4.91934528208445));
#11468=CARTESIAN_POINT('',(10.4270144578429,-3.53609615633055,4.91934528208444));
#11469=CARTESIAN_POINT('',(-10.5777124257746,3.53610097918737,4.91934528208445));
#11470=CARTESIAN_POINT('',(-10.5777124257746,-3.53609615633055,4.91934528208444));
#11471=CARTESIAN_POINT('',(10.4270144578429,3.53610097918737,4.91934528208444));
#11472=CARTESIAN_POINT('Origin',(10.4270144578429,3.53610097918737,9.71934528208445));
#11473=CARTESIAN_POINT('',(-16.37182497547,3.53610097918737,2.79386188249054));
#11474=CARTESIAN_POINT('',(-15.1031958253685,3.53610097918737,1.52523273238902));
#11475=CARTESIAN_POINT('',(-16.9375104004193,3.53610097918737,3.35954730743978));
#11476=CARTESIAN_POINT('',(-16.37182497547,3.53610097918737,3.92523273238902));
#11477=CARTESIAN_POINT('Origin',(-15.8061395505208,3.53610097918737,3.35954730743978));
#11478=CARTESIAN_POINT('',(-10.5777124257746,3.53610097918737,9.71934528208445));
#11479=CARTESIAN_POINT('',(-16.9375104004193,3.53610097918737,3.35954730743978));
#11480=CARTESIAN_POINT('',(10.4270144578429,3.53610097918737,9.71934528208445));
#11481=CARTESIAN_POINT('',(-13.97182497547,3.53610097918737,1.52523273238902));
#11482=CARTESIAN_POINT('',(-14.5375104004193,3.53610097918737,0.959547307439778));
#11483=CARTESIAN_POINT('Origin',(-14.5375104004193,3.53610097918737,2.09091815733826));
#11484=CARTESIAN_POINT('Origin',(10.4270144578429,-3.53609615633055,9.71934528208445));
#11485=CARTESIAN_POINT('',(-10.5777124257746,-3.53609615633055,9.71934528208445));
#11486=CARTESIAN_POINT('',(-10.5777124257746,-3.53609615633055,9.71934528208445));
#11487=CARTESIAN_POINT('',(10.4270144578429,-3.53609615633055,9.71934528208445));
#11488=CARTESIAN_POINT('Origin',(10.4270144578429,-3.53609615633055,9.71934528208445));
#11489=CARTESIAN_POINT('',(-16.37182497547,-3.53609615633055,3.92523273238902));
#11490=CARTESIAN_POINT('',(-16.9375104004193,-3.53609615633055,3.35954730743978));
#11491=CARTESIAN_POINT('Origin',(-15.8061395505208,-3.53609615633055,3.35954730743978));
#11492=CARTESIAN_POINT('',(-13.97182497547,-3.53609615633055,1.52523273238902));
#11493=CARTESIAN_POINT('Origin',(-14.5375104004193,-3.53609615633055,2.09091815733826));
#11494=CARTESIAN_POINT('',(-14.5375104004193,-3.53609615633055,0.959547307439778));
#11495=CARTESIAN_POINT('Origin',(-14.5375104004193,3.53610097918737,0.959547307439778));
#11496=CARTESIAN_POINT('',(-13.97182497547,-1.99999758857159,1.52523273238902));
#11497=CARTESIAN_POINT('',(-13.97182497547,-1.99999758857159,1.52523273238902));
#11498=CARTESIAN_POINT('',(-11.1433978507238,-1.99999758857159,4.3536598571352));
#11499=CARTESIAN_POINT('',(-14.5375104004193,-1.99999758857159,0.959547307439778));
#11500=CARTESIAN_POINT('',(-11.1433978507238,2.00000241142841,4.35365985713521));
#11501=CARTESIAN_POINT('',(-11.1433978507238,3.53610097918737,4.3536598571352));
#11502=CARTESIAN_POINT('',(-13.97182497547,2.00000241142841,1.52523273238902));
#11503=CARTESIAN_POINT('',(-14.5375104004193,2.00000241142841,0.959547307439778));
#11504=CARTESIAN_POINT('',(-13.97182497547,3.53610097918737,1.52523273238902));
#11505=CARTESIAN_POINT('Origin',(-16.9375104004193,-3.53609615633055,3.35954730743978));
#11506=CARTESIAN_POINT('',(-13.5433978507239,2.00000241142841,6.75365985713521));
#11507=CARTESIAN_POINT('',(-16.37182497547,2.00000241142841,3.92523273238902));
#11508=CARTESIAN_POINT('',(-19.7659375251655,2.00000241142841,0.531120182693588));
#11509=CARTESIAN_POINT('',(-13.5433978507239,-1.99999758857159,6.75365985713521));
#11510=CARTESIAN_POINT('',(-13.5433978507239,-3.53609615633055,6.75365985713521));
#11511=CARTESIAN_POINT('',(-16.37182497547,-1.99999758857159,3.92523273238902));
#11512=CARTESIAN_POINT('',(-19.7659375251655,-1.99999758857159,0.531120182693588));
#11513=CARTESIAN_POINT('',(-16.37182497547,-3.53609615633055,3.92523273238902));
#11514=CARTESIAN_POINT('',(-16.37182497547,2.00000241142841,3.92523273238902));
#11515=CARTESIAN_POINT('Origin',(-9.15718923943328,2.4114284077716E-6,-4.42077385354621));
#11516=CARTESIAN_POINT('',(-16.37182497547,2.00000241142841,2.79386188249054));
#11517=CARTESIAN_POINT('',(-15.1031958253685,2.00000241142841,1.52523273238902));
#11518=CARTESIAN_POINT('',(-9.15718923943328,2.00000241142841,-4.42077385354621));
#11519=CARTESIAN_POINT('',(-16.37182497547,3.53610097918737,2.79386188249054));
#11520=CARTESIAN_POINT('',(-15.1031958253685,2.00000241142841,1.52523273238902));
#11521=CARTESIAN_POINT('Origin',(-10.1492853010284,2.00000241142841,2.2281764575413));
#11522=CARTESIAN_POINT('',(-12.2747687006223,-1.99999758857159,4.35365985713521));
#11523=CARTESIAN_POINT('',(-13.5433978507238,-1.99999758857159,5.62228900723673));
#11524=CARTESIAN_POINT('',(-10.1492853010284,-1.99999758857159,2.2281764575413));
#11525=CARTESIAN_POINT('',(-13.5433978507238,2.00000241142841,5.62228900723673));
#11526=CARTESIAN_POINT('',(-13.5433978507238,2.00000241142841,5.62228900723673));
#11527=CARTESIAN_POINT('',(-12.2747687006223,2.00000241142841,4.35365985713521));
#11528=CARTESIAN_POINT('',(-10.1492853010284,2.00000241142841,2.2281764575413));
#11529=CARTESIAN_POINT('',(-12.2747687006223,2.00000241142841,4.35365985713521));
#11530=CARTESIAN_POINT('Origin',(-15.8061395505208,-1.99999758857159,-3.42867779195108));
#11531=CARTESIAN_POINT('Origin',(-15.8061395505208,-1.99999758857159,3.35954730743978));
#11532=CARTESIAN_POINT('Origin',(-12.9777124257746,-1.99999758857159,6.18797443218597));
#11533=CARTESIAN_POINT('Origin',(-11.7090832756731,-1.99999758857159,4.91934528208444));
#11534=CARTESIAN_POINT('Origin',(-14.5375104004193,-1.99999758857159,2.09091815733826));
#11535=CARTESIAN_POINT('Origin',(-15.8061395505208,2.00000241142841,-3.42867779195108));
#11536=CARTESIAN_POINT('Origin',(-15.8061395505208,2.00000241142841,3.35954730743978));
#11537=CARTESIAN_POINT('Origin',(-14.5375104004193,2.00000241142841,2.09091815733826));
#11538=CARTESIAN_POINT('Origin',(-11.7090832756731,2.00000241142841,4.91934528208444));
#11539=CARTESIAN_POINT('Origin',(-12.9777124257746,2.00000241142841,6.18797443218597));
#11540=CARTESIAN_POINT('Origin',(-14.6061395505208,-4.33609615633055,3.29091815733825));
#11541=CARTESIAN_POINT('Origin',(-14.6061395505208,4.33590384366945,3.29091815733825));
#11542=CARTESIAN_POINT('Origin',(-12.9777124257746,2.00000241142841,6.18797443218597));
#11543=CARTESIAN_POINT('Origin',(-15.8061395505208,2.4114284077716E-6,3.35954730743978));
#11544=CARTESIAN_POINT('Origin',(-15.8061395505208,2.4114284077716E-6,3.35954730743978));
#11545=CARTESIAN_POINT('Origin',(-14.5375104004193,2.4114284077716E-6,2.09091815733826));
#11546=CARTESIAN_POINT('Origin',(-14.5375104004193,2.4114284077716E-6,2.09091815733826));
#11547=CARTESIAN_POINT('Origin',(-11.7090832756731,3.53610097918737,4.91934528208444));
#11548=CARTESIAN_POINT('Origin',(-0.177712466787677,2.4114284077716E-6,
40.5587029190994));
#11549=CARTESIAN_POINT('',(-3.73255732111315,-3.53609615633055,40.5587029190994));
#11550=CARTESIAN_POINT('',(3.37713238753779,-3.53609615633055,40.5587029190994));
#11551=CARTESIAN_POINT('',(5.77713238753779,-3.53609615633055,40.5587029190994));
#11552=CARTESIAN_POINT('',(3.37713238753779,3.53610097918737,40.5587029190994));
#11553=CARTESIAN_POINT('',(3.37713238753779,3.53610097918737,40.5587029190994));
#11554=CARTESIAN_POINT('',(-3.73255732111315,3.53610097918737,40.5587029190994));
#11555=CARTESIAN_POINT('',(5.77713238753779,3.53610097918737,40.5587029190994));
#11556=CARTESIAN_POINT('',(-3.73255732111315,-3.53609615633055,40.5587029190994));
#11557=CARTESIAN_POINT('Origin',(5.77713238753779,-3.53609615633055,1.29011815733825));
#11558=CARTESIAN_POINT('',(5.77713238753779,-3.53609615633055,38.1587029190994));
#11559=CARTESIAN_POINT('',(5.77713238753779,-3.53609615633055,1.29011815733825));
#11560=CARTESIAN_POINT('Origin',(3.37713238753779,-3.53609615633055,38.1587029190994));
#11561=CARTESIAN_POINT('',(-6.13255732111315,-3.53609615633055,38.1587029190994));
#11562=CARTESIAN_POINT('Origin',(-3.73255732111315,-3.53609615633055,38.1587029190994));
#11563=CARTESIAN_POINT('',(-6.13255732111315,-3.53609615633055,1.29011815733825));
#11564=CARTESIAN_POINT('Origin',(5.77713238753779,3.53610097918737,1.29011815733825));
#11565=CARTESIAN_POINT('',(5.77713238753779,3.53610097918737,38.1587029190994));
#11566=CARTESIAN_POINT('',(5.77713238753779,3.53610097918737,1.29011815733825));
#11567=CARTESIAN_POINT('',(5.77713238753779,-3.53609615633055,38.1587029190994));
#11568=CARTESIAN_POINT('Origin',(5.77713238753779,3.53610097918737,1.29011815733825));
#11569=CARTESIAN_POINT('Origin',(3.37713238753779,3.53610097918737,38.1587029190994));
#11570=CARTESIAN_POINT('',(-6.13255732111315,3.53610097918737,38.1587029190994));
#11571=CARTESIAN_POINT('',(-6.13255732111315,3.53610097918737,1.29011815733825));
#11572=CARTESIAN_POINT('Origin',(-3.73255732111315,3.53610097918737,38.1587029190994));
#11573=CARTESIAN_POINT('Origin',(-6.13255732111315,3.53610097918737,1.29011815733825));
#11574=CARTESIAN_POINT('',(-6.13255732111315,3.53610097918737,38.1587029190994));
#11575=CARTESIAN_POINT('Origin',(3.37713238753779,2.4114284077716E-6,38.1587029190994));
#11576=CARTESIAN_POINT('Origin',(-3.73255732111315,2.4114284077716E-6,38.1587029190994));
#11577=CARTESIAN_POINT('Origin',(-4.21925722373829,20.,17.6406068922372));
#11578=CARTESIAN_POINT('Origin',(-4.21925722373829,20.,17.6406068922372));
#11579=CARTESIAN_POINT('Origin',(9.60397861284329,20.,11.8903072744979));
#11580=CARTESIAN_POINT('Origin',(9.60397861284329,20.,11.8903072744979));
#11581=CARTESIAN_POINT('',(6.42417721261744,20.,14.4149297172206));
#11582=CARTESIAN_POINT('Origin',(9.60397861284329,20.,11.8903072744979));
#11583=CARTESIAN_POINT('',(6.42417721261744,20.,14.4149297172206));
#11584=CARTESIAN_POINT('Origin',(-10.8056176096432,20.,28.0946289238114));
#11585=CARTESIAN_POINT('Origin',(-10.8056176096432,20.,28.0946289238114));
#11586=CARTESIAN_POINT('',(0.,0.,0.));
#11587=CARTESIAN_POINT('',(0.,0.,0.));
#11588=CARTESIAN_POINT('Origin',(0.,0.,9.72414336253035));
#11589=CARTESIAN_POINT('',(-1.825,-2.23498040844392E-16,9.72414336253035));
#11590=CARTESIAN_POINT('Origin',(0.,0.,9.72414336253035));
#11591=CARTESIAN_POINT('',(-1.825,-2.23498040844392E-16,29.4341433625304));
#11592=CARTESIAN_POINT('',(-1.825,-2.23498040844392E-16,9.72414336253035));
#11593=CARTESIAN_POINT('Origin',(0.,0.,29.4341433625304));
#11594=CARTESIAN_POINT('Origin',(-2.92,4.33680868994202E-16,1.69414336253035));
#11595=CARTESIAN_POINT('',(-1.46,-1.095,1.69414336253035));
#11596=CARTESIAN_POINT('Origin',(-1.46,4.33680868994202E-16,1.69414336253035));
#11597=CARTESIAN_POINT('',(1.46,-1.095,1.69414336253035));
#11598=CARTESIAN_POINT('',(-2.92,-1.095,1.69414336253035));
#11599=CARTESIAN_POINT('Origin',(1.46,0.,1.69414336253035));
#11600=CARTESIAN_POINT('Origin',(0.,0.,29.4341433625304));
#11601=CARTESIAN_POINT('',(2.92,-3.57596865351027E-16,3.88414336253035));
#11602=CARTESIAN_POINT('Origin',(0.,0.,3.88414336253035));
#11603=CARTESIAN_POINT('',(2.92,-3.57596865351027E-16,29.4341433625304));
#11604=CARTESIAN_POINT('',(2.92,-3.57596865351027E-16,29.4341433625304));
#11605=CARTESIAN_POINT('Origin',(0.,0.,29.4341433625304));
#11606=CARTESIAN_POINT('Origin',(0.,0.,3.88414336253035));
#11607=CARTESIAN_POINT('',(-1.46,-2.19,3.88414336253035));
#11608=CARTESIAN_POINT('',(-1.46,2.19,3.88414336253035));
#11609=CARTESIAN_POINT('',(-1.46,2.19,3.88414336253035));
#11610=CARTESIAN_POINT('',(1.46,-2.19,3.88414336253035));
#11611=CARTESIAN_POINT('',(1.46,-2.19,3.88414336253035));
#11612=CARTESIAN_POINT('',(1.46,2.19,3.88414336253035));
#11613=CARTESIAN_POINT('',(1.46,2.19,3.88414336253035));
#11614=CARTESIAN_POINT('',(1.46,2.19,3.88414336253035));
#11615=CARTESIAN_POINT('Origin',(0.,0.,29.4341433625304));
#11616=CARTESIAN_POINT('Origin',(-1.46,2.19,-0.495856637469653));
#11617=CARTESIAN_POINT('',(-1.46,2.19,1.69414336253035));
#11618=CARTESIAN_POINT('',(-1.46,-2.19,1.69414336253035));
#11619=CARTESIAN_POINT('Origin',(-1.46,0.,1.69414336253035));
#11620=CARTESIAN_POINT('',(-1.46,-2.19,-0.495856637469653));
#11621=CARTESIAN_POINT('',(-1.46,2.19,-0.495856637469653));
#11622=CARTESIAN_POINT('Origin',(1.46,2.19,-0.495856637469653));
#11623=CARTESIAN_POINT('',(1.46,2.19,1.69414336253035));
#11624=CARTESIAN_POINT('',(1.46,2.19,-0.495856637469653));
#11625=CARTESIAN_POINT('',(-1.46,2.19,1.69414336253035));
#11626=CARTESIAN_POINT('Origin',(1.46,2.19,-0.495856637469653));
#11627=CARTESIAN_POINT('',(1.46,-2.19,1.69414336253035));
#11628=CARTESIAN_POINT('',(1.46,-2.19,-0.495856637469653));
#11629=CARTESIAN_POINT('Origin',(1.46,0.,1.69414336253035));
#11630=CARTESIAN_POINT('Origin',(1.46,-2.19,-0.495856637469653));
#11631=CARTESIAN_POINT('',(1.46,-2.19,1.69414336253035));
#11632=CARTESIAN_POINT('Origin',(0.,0.,1.69414336253035));
#11633=CARTESIAN_POINT('Origin',(0.,0.,9.72414336253035));
#11634=CARTESIAN_POINT('',(0.,0.,0.));
#11635=CARTESIAN_POINT('Origin',(-0.73,-4.33680868994202E-16,23.652));
#11636=CARTESIAN_POINT('',(-0.73,-0.729999999999999,23.652));
#11637=CARTESIAN_POINT('Origin',(-0.73,-4.33680868994202E-16,23.652));
#11638=CARTESIAN_POINT('',(0.73,-0.729999999999999,23.652));
#11639=CARTESIAN_POINT('',(-0.73,-0.729999999999999,23.652));
#11640=CARTESIAN_POINT('Origin',(0.73,0.,23.652));
#11641=CARTESIAN_POINT('Origin',(-4.85950360212944,-8.67361737988404E-16,
23.652));
#11642=CARTESIAN_POINT('',(-0.73,-1.2775,22.9451805393171));
#11643=CARTESIAN_POINT('',(-0.73,1.2775,22.9451805393171));
#11644=CARTESIAN_POINT('Origin',(-0.73,-4.33680868994202E-16,23.652));
#11645=CARTESIAN_POINT('',(0.73,-1.2775,22.9451805393171));
#11646=CARTESIAN_POINT('',(-4.85950360212944,-1.2775,22.9451805393171));
#11647=CARTESIAN_POINT('',(0.73,1.2775,22.9451805393171));
#11648=CARTESIAN_POINT('Origin',(0.73,0.,23.652));
#11649=CARTESIAN_POINT('',(-4.85950360212944,1.2775,22.9451805393172));
#11650=CARTESIAN_POINT('Origin',(0.,0.,20.44));
#11651=CARTESIAN_POINT('',(1.825,-2.23498040844392E-16,0.));
#11652=CARTESIAN_POINT('Origin',(0.,0.,0.));
#11653=CARTESIAN_POINT('',(1.825,-2.23498040844392E-16,20.44));
#11654=CARTESIAN_POINT('',(1.825,-2.23498040844392E-16,20.44));
#11655=CARTESIAN_POINT('Origin',(0.,0.,20.44));
#11656=CARTESIAN_POINT('Origin',(0.,0.,20.44));
#11657=CARTESIAN_POINT('',(0.73,1.2775,20.44));
#11658=CARTESIAN_POINT('',(-0.73,1.2775,20.44));
#11659=CARTESIAN_POINT('',(-0.73,1.2775,20.44));
#11660=CARTESIAN_POINT('',(0.73,-1.2775,20.44));
#11661=CARTESIAN_POINT('',(0.73,1.2775,20.44));
#11662=CARTESIAN_POINT('',(-0.73,-1.2775,20.44));
#11663=CARTESIAN_POINT('',(-0.73,-1.2775,20.44));
#11664=CARTESIAN_POINT('',(-0.73,1.2775,20.44));
#11665=CARTESIAN_POINT('Origin',(0.,0.,0.));
#11666=CARTESIAN_POINT('Origin',(0.73,1.2775,23.652));
#11667=CARTESIAN_POINT('',(0.73,1.2775,23.652));
#11668=CARTESIAN_POINT('',(0.73,-1.2775,23.652));
#11669=CARTESIAN_POINT('Origin',(-0.73,1.2775,23.652));
#11670=CARTESIAN_POINT('',(-0.73,1.2775,23.652));
#11671=CARTESIAN_POINT('Origin',(-0.73,1.2775,23.652));
#11672=CARTESIAN_POINT('',(-0.73,-1.2775,23.652));
#11673=CARTESIAN_POINT('Origin',(-0.73,-1.2775,23.652));
#11674=CARTESIAN_POINT('',(-13.1648862463908,-2.12457642057912,-6.69250946692208));
#11675=CARTESIAN_POINT('',(-13.1648862463873,-2.12457642056474,18.3499596826252));
#11676=CARTESIAN_POINT('',(0.,0.,0.));
#11677=CARTESIAN_POINT('',(0.,0.,0.));
#11678=CARTESIAN_POINT('Origin',(6.03700957585037E-17,-6.47376725810661E-18,
5.59782889707835));
#11679=CARTESIAN_POINT('',(-1.825,-2.29971808102499E-16,5.59782889707835));
#11680=CARTESIAN_POINT('Origin',(6.03700957585037E-17,-6.47376725810661E-18,
5.59782889707835));
#11681=CARTESIAN_POINT('',(-1.825,-2.29971808102499E-16,25.3078288970784));
#11682=CARTESIAN_POINT('',(-1.825,-2.29971808102499E-16,5.59782889707835));
#11683=CARTESIAN_POINT('Origin',(6.03700957585037E-17,-6.47376725810661E-18,
25.3078288970784));
#11684=CARTESIAN_POINT('Origin',(-2.92,3.76068899267196E-16,1.21782889707835));
#11685=CARTESIAN_POINT('',(-1.46,-1.095,1.21782889707835));
#11686=CARTESIAN_POINT('Origin',(-1.46,2.17775382084312E-16,1.21782889707835));
#11687=CARTESIAN_POINT('',(1.46,-1.095,1.21782889707835));
#11688=CARTESIAN_POINT('',(-2.92,-1.095,1.21782889707835));
#11689=CARTESIAN_POINT('Origin',(1.46,-9.88116522814554E-17,1.21782889707835));
#11690=CARTESIAN_POINT('Origin',(6.03700957585037E-17,-6.47376725810661E-18,
25.3078288970784));
#11691=CARTESIAN_POINT('',(2.92,-3.64070632609134E-16,3.40782889707835));
#11692=CARTESIAN_POINT('Origin',(6.03700957585037E-17,-6.47376725810661E-18,
3.40782889707835));
#11693=CARTESIAN_POINT('',(2.92,-3.64070632609134E-16,25.3078288970784));
#11694=CARTESIAN_POINT('',(2.92,-3.64070632609134E-16,25.3078288970784));
#11695=CARTESIAN_POINT('Origin',(6.03700957585037E-17,-6.47376725810661E-18,
25.3078288970784));
#11696=CARTESIAN_POINT('Origin',(6.03700957585037E-17,-6.47376725810661E-18,
3.40782889707835));
#11697=CARTESIAN_POINT('',(-1.46,-2.19,3.40782889707835));
#11698=CARTESIAN_POINT('',(-1.46,2.19,3.40782889707835));
#11699=CARTESIAN_POINT('',(-1.46,2.19,3.40782889707835));
#11700=CARTESIAN_POINT('',(1.46,-2.19,3.40782889707835));
#11701=CARTESIAN_POINT('',(1.46,-2.19,3.40782889707835));
#11702=CARTESIAN_POINT('',(1.46,2.19,3.40782889707835));
#11703=CARTESIAN_POINT('',(1.46,2.19,3.40782889707835));
#11704=CARTESIAN_POINT('',(1.46,2.19,3.40782889707835));
#11705=CARTESIAN_POINT('Origin',(6.03700957585037E-17,-6.47376725810661E-18,
25.3078288970784));
#11706=CARTESIAN_POINT('Origin',(-1.46,2.19,-0.972171102921649));
#11707=CARTESIAN_POINT('',(-1.46,2.19,1.21782889707835));
#11708=CARTESIAN_POINT('',(-1.46,-2.19,1.21782889707835));
#11709=CARTESIAN_POINT('Origin',(-1.46,-6.47376725810661E-18,1.21782889707835));
#11710=CARTESIAN_POINT('',(-1.46,-2.19,-0.972171102921649));
#11711=CARTESIAN_POINT('',(-1.46,2.19,-0.972171102921649));
#11712=CARTESIAN_POINT('Origin',(1.46,2.19,-0.972171102921649));
#11713=CARTESIAN_POINT('',(1.46,2.19,1.21782889707835));
#11714=CARTESIAN_POINT('',(1.46,2.19,-0.972171102921649));
#11715=CARTESIAN_POINT('',(-1.46,2.19,1.21782889707835));
#11716=CARTESIAN_POINT('Origin',(1.46,2.19,-0.972171102921649));
#11717=CARTESIAN_POINT('',(1.46,-2.19,1.21782889707835));
#11718=CARTESIAN_POINT('',(1.46,-2.19,-0.972171102921649));
#11719=CARTESIAN_POINT('Origin',(1.46,-6.47376725810661E-18,1.21782889707835));
#11720=CARTESIAN_POINT('Origin',(1.46,-2.19,-0.972171102921649));
#11721=CARTESIAN_POINT('',(1.46,-2.19,1.21782889707835));
#11722=CARTESIAN_POINT('Origin',(6.03700957585037E-17,-6.47376725810661E-18,
1.21782889707835));
#11723=CARTESIAN_POINT('Origin',(6.03700957585037E-17,-6.47376725810661E-18,
5.59782889707835));
#11724=CARTESIAN_POINT('',(0.,0.,0.));
#11725=CARTESIAN_POINT('Origin',(-0.73,-5.37449520079003E-16,21.462));
#11726=CARTESIAN_POINT('',(-0.73,-0.730000000000002,21.462));
#11727=CARTESIAN_POINT('Origin',(-0.73,-5.37449520079003E-16,21.462));
#11728=CARTESIAN_POINT('',(0.73,-0.730000000000002,21.462));
#11729=CARTESIAN_POINT('',(-0.73,-0.730000000000002,21.462));
#11730=CARTESIAN_POINT('Origin',(0.73,-3.56542643298565E-16,21.462));
#11731=CARTESIAN_POINT('Origin',(-4.85950360212944,-1.04913143741791E-15,
21.462));
#11732=CARTESIAN_POINT('',(-0.73,-1.2775,20.7551805393172));
#11733=CARTESIAN_POINT('',(-0.73,1.2775,20.7551805393172));
#11734=CARTESIAN_POINT('Origin',(-0.73,-5.37449520079003E-16,21.462));
#11735=CARTESIAN_POINT('',(0.73,-1.2775,20.7551805393172));
#11736=CARTESIAN_POINT('',(-4.85950360212944,-1.2775,20.7551805393172));
#11737=CARTESIAN_POINT('',(0.73,1.2775,20.7551805393172));
#11738=CARTESIAN_POINT('Origin',(0.73,-3.56542643298565E-16,21.462));
#11739=CARTESIAN_POINT('',(-4.85950360212944,1.2775,20.7551805393172));
#11740=CARTESIAN_POINT('Origin',(0.,0.,18.25));
#11741=CARTESIAN_POINT('',(1.825,-2.23498040844392E-16,-2.22044604925031E-15));
#11742=CARTESIAN_POINT('Origin',(0.,0.,0.));
#11743=CARTESIAN_POINT('',(1.825,-2.23498040844392E-16,18.25));
#11744=CARTESIAN_POINT('',(1.825,-2.23498040844392E-16,18.25));
#11745=CARTESIAN_POINT('Origin',(0.,0.,18.25));
#11746=CARTESIAN_POINT('Origin',(0.,0.,18.25));
#11747=CARTESIAN_POINT('',(0.73,1.2775,18.25));
#11748=CARTESIAN_POINT('',(-0.73,1.2775,18.25));
#11749=CARTESIAN_POINT('',(-0.73,1.2775,18.25));
#11750=CARTESIAN_POINT('',(0.73,-1.2775,18.25));
#11751=CARTESIAN_POINT('',(0.73,1.2775,18.25));
#11752=CARTESIAN_POINT('',(-0.73,-1.2775,18.25));
#11753=CARTESIAN_POINT('',(-0.73,-1.2775,18.25));
#11754=CARTESIAN_POINT('',(-0.73,1.2775,18.25));
#11755=CARTESIAN_POINT('Origin',(0.,0.,0.));
#11756=CARTESIAN_POINT('Origin',(0.73,1.2775,21.462));
#11757=CARTESIAN_POINT('',(0.73,1.2775,21.462));
#11758=CARTESIAN_POINT('',(0.73,-1.2775,21.462));
#11759=CARTESIAN_POINT('Origin',(-0.73,1.2775,21.462));
#11760=CARTESIAN_POINT('',(-0.73,1.2775,21.462));
#11761=CARTESIAN_POINT('Origin',(-0.73,1.2775,21.462));
#11762=CARTESIAN_POINT('',(-0.73,-1.2775,21.462));
#11763=CARTESIAN_POINT('Origin',(-0.73,-1.2775,21.462));
#11764=CARTESIAN_POINT('',(-13.1648862463908,-2.12457642057906,-6.69250946692213));
#11765=CARTESIAN_POINT('',(-13.1648862461968,-2.12457642043762,18.3653194301352));
#11766=CARTESIAN_POINT('',(0.,0.,0.));
#11767=CARTESIAN_POINT('',(0.,0.,0.));
#11768=CARTESIAN_POINT('Origin',(0.,0.,3.));
#11769=CARTESIAN_POINT('',(-2.5,-3.06161699786838E-16,3.));
#11770=CARTESIAN_POINT('Origin',(0.,0.,3.));
#11771=CARTESIAN_POINT('',(-2.5,-3.06161699786838E-16,30.));
#11772=CARTESIAN_POINT('',(-2.5,-3.06161699786838E-16,3.));
#11773=CARTESIAN_POINT('Origin',(0.,0.,30.));
#11774=CARTESIAN_POINT('Origin',(-4.,4.33680868994202E-16,-3.));
#11775=CARTESIAN_POINT('',(-2.,-1.5,-3.));
#11776=CARTESIAN_POINT('Origin',(-2.,2.16840434497101E-16,-3.));
#11777=CARTESIAN_POINT('',(2.,-1.5,-3.));
#11778=CARTESIAN_POINT('',(-4.,-1.5,-3.));
#11779=CARTESIAN_POINT('Origin',(2.,-2.16840434497101E-16,-3.));
#11780=CARTESIAN_POINT('Origin',(0.,0.,30.));
#11781=CARTESIAN_POINT('',(4.,-4.89858719658941E-16,0.));
#11782=CARTESIAN_POINT('Origin',(0.,0.,0.));
#11783=CARTESIAN_POINT('',(4.,-4.89858719658941E-16,30.));
#11784=CARTESIAN_POINT('',(4.,-4.89858719658941E-16,30.));
#11785=CARTESIAN_POINT('Origin',(0.,0.,30.));
#11786=CARTESIAN_POINT('Origin',(0.,0.,0.));
#11787=CARTESIAN_POINT('',(-2.,-3.,0.));
#11788=CARTESIAN_POINT('',(-2.,3.,0.));
#11789=CARTESIAN_POINT('',(-2.,3.,0.));
#11790=CARTESIAN_POINT('',(2.,-3.,0.));
#11791=CARTESIAN_POINT('',(2.,-3.,0.));
#11792=CARTESIAN_POINT('',(2.,3.,0.));
#11793=CARTESIAN_POINT('',(2.,3.,0.));
#11794=CARTESIAN_POINT('',(2.,3.,0.));
#11795=CARTESIAN_POINT('Origin',(0.,0.,30.));
#11796=CARTESIAN_POINT('Origin',(-2.,3.,-6.));
#11797=CARTESIAN_POINT('',(-2.,3.,-3.));
#11798=CARTESIAN_POINT('',(-2.,-3.,-3.));
#11799=CARTESIAN_POINT('Origin',(-2.,0.,-3.));
#11800=CARTESIAN_POINT('',(-2.,-3.,-6.));
#11801=CARTESIAN_POINT('',(-2.,3.,-6.));
#11802=CARTESIAN_POINT('Origin',(2.,3.,-6.));
#11803=CARTESIAN_POINT('',(2.,3.,-3.));
#11804=CARTESIAN_POINT('',(2.,3.,-6.));
#11805=CARTESIAN_POINT('',(-2.,3.,-3.));
#11806=CARTESIAN_POINT('Origin',(2.,3.,-6.));
#11807=CARTESIAN_POINT('',(2.,-3.,-3.));
#11808=CARTESIAN_POINT('',(2.,-3.,-6.));
#11809=CARTESIAN_POINT('Origin',(2.,0.,-3.));
#11810=CARTESIAN_POINT('Origin',(2.,-3.,-6.));
#11811=CARTESIAN_POINT('',(2.,-3.,-3.));
#11812=CARTESIAN_POINT('Origin',(0.,0.,-3.));
#11813=CARTESIAN_POINT('Origin',(0.,0.,3.));
#11814=CARTESIAN_POINT('',(0.,0.,0.));
#11815=CARTESIAN_POINT('Origin',(-1.,-6.50521303491303E-16,29.4));
#11816=CARTESIAN_POINT('',(-1.,-1.,29.4));
#11817=CARTESIAN_POINT('Origin',(-1.,-6.50521303491303E-16,29.4));
#11818=CARTESIAN_POINT('',(1.00000000000001,-1.,29.4));
#11819=CARTESIAN_POINT('',(-1.,-1.,29.4));
#11820=CARTESIAN_POINT('Origin',(1.00000000000001,-4.33680868994202E-16,
29.4));
#11821=CARTESIAN_POINT('Origin',(-6.6568542494924,-2.16840434497101E-16,
29.4));
#11822=CARTESIAN_POINT('',(-1.,-1.75000000000001,28.4317541634482));
#11823=CARTESIAN_POINT('',(-1.,1.75000000000001,28.4317541634482));
#11824=CARTESIAN_POINT('Origin',(-1.,-6.50521303491303E-16,29.4));
#11825=CARTESIAN_POINT('',(1.,-1.75000000000001,28.4317541634482));
#11826=CARTESIAN_POINT('',(-6.6568542494924,-1.75,28.4317541634482));
#11827=CARTESIAN_POINT('',(1.,1.75000000000001,28.4317541634482));
#11828=CARTESIAN_POINT('Origin',(1.00000000000001,-4.33680868994202E-16,
29.4));
#11829=CARTESIAN_POINT('',(-6.65685424949239,1.75000000000001,28.4317541634482));
#11830=CARTESIAN_POINT('Origin',(0.,0.,25.));
#11831=CARTESIAN_POINT('',(2.50000000000001,-3.06161699786839E-16,0.));
#11832=CARTESIAN_POINT('Origin',(0.,0.,0.));
#11833=CARTESIAN_POINT('',(2.50000000000001,-3.06161699786839E-16,25.));
#11834=CARTESIAN_POINT('',(2.50000000000001,-3.06161699786839E-16,25.));
#11835=CARTESIAN_POINT('Origin',(0.,0.,25.));
#11836=CARTESIAN_POINT('Origin',(0.,0.,25.));
#11837=CARTESIAN_POINT('',(1.,1.75000000000001,25.));
#11838=CARTESIAN_POINT('',(-1.,1.75000000000001,25.));
#11839=CARTESIAN_POINT('',(-1.,1.75000000000001,25.));
#11840=CARTESIAN_POINT('',(1.,-1.75000000000001,25.));
#11841=CARTESIAN_POINT('',(1.,1.75000000000001,25.));
#11842=CARTESIAN_POINT('',(-1.,-1.75000000000001,25.));
#11843=CARTESIAN_POINT('',(-1.,-1.75000000000001,25.));
#11844=CARTESIAN_POINT('',(-1.,1.75000000000001,25.));
#11845=CARTESIAN_POINT('Origin',(0.,0.,0.));
#11846=CARTESIAN_POINT('Origin',(1.,1.75000000000001,29.4));
#11847=CARTESIAN_POINT('',(1.,1.75000000000001,29.4));
#11848=CARTESIAN_POINT('',(1.,-1.75000000000001,29.4));
#11849=CARTESIAN_POINT('Origin',(-1.,1.75000000000001,29.4));
#11850=CARTESIAN_POINT('',(-1.,1.75000000000001,29.4));
#11851=CARTESIAN_POINT('Origin',(-1.,1.75000000000001,29.4));
#11852=CARTESIAN_POINT('',(-1.,-1.75000000000001,29.4));
#11853=CARTESIAN_POINT('Origin',(-1.,-1.75000000000001,29.4));
#11854=CARTESIAN_POINT('',(0.,0.,0.));
#11855=CARTESIAN_POINT('Origin',(6.,7.84619407771256,5.84619407771256));
#11856=CARTESIAN_POINT('',(5.,7.84619407771256,4.84619407771256));
#11857=CARTESIAN_POINT('Origin',(5.,7.84619407771256,5.84619407771256));
#11858=CARTESIAN_POINT('',(6.,7.84619407771256,4.84619407771256));
#11859=CARTESIAN_POINT('',(6.,7.84619407771256,4.84619407771256));
#11860=CARTESIAN_POINT('Origin',(6.,7.84619407771256,5.84619407771256));
#11861=CARTESIAN_POINT('Origin',(6.,7.84619407771256,5.84619407771256));
#11862=CARTESIAN_POINT('',(-6.,7.84619407771256,4.84619407771256));
#11863=CARTESIAN_POINT('Origin',(-6.,7.84619407771256,5.84619407771256));
#11864=CARTESIAN_POINT('',(-5.,7.84619407771256,4.84619407771256));
#11865=CARTESIAN_POINT('',(6.,7.84619407771256,4.84619407771256));
#11866=CARTESIAN_POINT('Origin',(-5.,7.84619407771256,5.84619407771256));
#11867=CARTESIAN_POINT('Origin',(6.,7.84619407771256,5.84619407771256));
#11868=CARTESIAN_POINT('',(-2.5,7.84619407771256,4.84619407771256));
#11869=CARTESIAN_POINT('Origin',(-2.5,7.84619407771256,5.84619407771256));
#11870=CARTESIAN_POINT('',(2.5,7.84619407771256,4.84619407771256));
#11871=CARTESIAN_POINT('',(6.,7.84619407771256,4.84619407771256));
#11872=CARTESIAN_POINT('Origin',(2.5,7.84619407771256,5.84619407771256));
#11873=CARTESIAN_POINT('Origin',(0.,7.90685424949238,7.90685424949238));
#11874=CARTESIAN_POINT('',(2.5,7.65685424949238,8.15685424949238));
#11875=CARTESIAN_POINT('',(2.5,10.1568542494924,5.65685424949238));
#11876=CARTESIAN_POINT('',(2.5,7.90685424949238,7.90685424949238));
#11877=CARTESIAN_POINT('',(5.,7.65685424949238,8.15685424949238));
#11878=CARTESIAN_POINT('',(-5.,7.65685424949238,8.15685424949238));
#11879=CARTESIAN_POINT('',(5.,10.1568542494924,5.65685424949238));
#11880=CARTESIAN_POINT('',(5.,7.65685424949238,8.15685424949238));
#11881=CARTESIAN_POINT('',(5.,10.1568542494924,5.65685424949238));
#11882=CARTESIAN_POINT('Origin',(5.,2.,2.5));
#11883=CARTESIAN_POINT('',(5.,0.,2.5));
#11884=CARTESIAN_POINT('',(5.,0.,-2.5));
#11885=CARTESIAN_POINT('',(5.,0.,2.5));
#11886=CARTESIAN_POINT('',(5.,2.,-2.5));
#11887=CARTESIAN_POINT('',(5.,2.,-2.5));
#11888=CARTESIAN_POINT('',(5.,10.1568542494924,5.65685424949238));
#11889=CARTESIAN_POINT('',(5.,2.,2.5));
#11890=CARTESIAN_POINT('',(5.,7.65685424949238,8.15685424949238));
#11891=CARTESIAN_POINT('',(5.,2.,2.5));
#11892=CARTESIAN_POINT('Origin',(-5.,2.,-2.5));
#11893=CARTESIAN_POINT('',(-5.,0.,-2.5));
#11894=CARTESIAN_POINT('',(-5.,0.,-2.5));
#11895=CARTESIAN_POINT('',(-5.,2.,-2.5));
#11896=CARTESIAN_POINT('',(-5.,2.,-2.5));
#11897=CARTESIAN_POINT('',(-5.,2.,-2.5));
#11898=CARTESIAN_POINT('Origin',(-5.,2.,2.5));
#11899=CARTESIAN_POINT('',(-5.,0.,2.5));
#11900=CARTESIAN_POINT('',(-5.,0.,2.5));
#11901=CARTESIAN_POINT('',(-5.,2.,2.5));
#11902=CARTESIAN_POINT('',(-5.,2.,2.5));
#11903=CARTESIAN_POINT('',(-5.,7.65685424949238,8.15685424949238));
#11904=CARTESIAN_POINT('',(-5.,7.65685424949238,8.15685424949238));
#11905=CARTESIAN_POINT('',(-5.,10.1568542494924,5.65685424949238));
#11906=CARTESIAN_POINT('',(-5.,10.1568542494924,5.65685424949238));
#11907=CARTESIAN_POINT('',(-5.,10.1568542494924,5.65685424949238));
#11908=CARTESIAN_POINT('Origin',(-5.,2.,2.5));
#11909=CARTESIAN_POINT('',(-5.,0.,2.5));
#11910=CARTESIAN_POINT('',(-5.,2.,2.5));
#11911=CARTESIAN_POINT('Origin',(0.,0.,0.));
#11912=CARTESIAN_POINT('Origin',(-5.,7.65685424949238,8.15685424949238));
#11913=CARTESIAN_POINT('',(2.5,2.35355339059327,2.85355339059327));
#11914=CARTESIAN_POINT('',(2.5,12.9601551083915,13.4601551083915));
#11915=CARTESIAN_POINT('',(-2.5,2.35355339059327,2.85355339059327));
#11916=CARTESIAN_POINT('',(-2.5,2.35355339059327,2.85355339059327));
#11917=CARTESIAN_POINT('',(-2.5,7.65685424949238,8.15685424949238));
#11918=CARTESIAN_POINT('',(-2.5,12.9601551083915,13.4601551083915));
#11919=CARTESIAN_POINT('',(-5.,7.65685424949238,8.15685424949238));
#11920=CARTESIAN_POINT('Origin',(5.,10.1568542494924,5.65685424949238));
#11921=CARTESIAN_POINT('',(2.5,4.85355339059327,0.353553390593271));
#11922=CARTESIAN_POINT('',(-2.5,4.85355339059327,0.353553390593271));
#11923=CARTESIAN_POINT('',(-2.5,4.85355339059327,0.353553390593271));
#11924=CARTESIAN_POINT('',(2.5,15.4601551083915,10.9601551083915));
#11925=CARTESIAN_POINT('',(-2.5,10.1568542494924,5.65685424949238));
#11926=CARTESIAN_POINT('',(5.,10.1568542494924,5.65685424949238));
#11927=CARTESIAN_POINT('',(-2.5,15.4601551083915,10.9601551083915));
#11928=CARTESIAN_POINT('Origin',(0.,7.90685424949238,7.90685424949238));
#11929=CARTESIAN_POINT('',(-2.5,7.90685424949238,7.90685424949238));
#11930=CARTESIAN_POINT('Origin',(2.5,1.77981522089254,24.6404949958904));
#11931=CARTESIAN_POINT('',(2.5,-8.82678649690568,14.0338932780922));
#11932=CARTESIAN_POINT('Origin',(-2.5,1.77981522089254,24.6404949958904));
#11933=CARTESIAN_POINT('',(-2.5,-8.82678649690568,14.0338932780922));
#11934=CARTESIAN_POINT('Origin',(-2.5,-8.82678649690568,14.0338932780922));
#11935=CARTESIAN_POINT('Origin',(-6.,7.84619407771256,5.84619407771256));
#11936=CARTESIAN_POINT('Origin',(6.,7.84619407771256,5.84619407771256));
#11937=CARTESIAN_POINT('',(-2.75679846963225,1.1523417603065,21.5));
#11938=CARTESIAN_POINT('',(-2.7567984695596,1.15234176026346,38.1907095183999));
#11939=CARTESIAN_POINT('',(-2.75679846963225,-6.67018106606782,12.6221701853264));
#11940=CARTESIAN_POINT('',(0.,0.,0.));
#11941=CARTESIAN_POINT('Origin',(26.,6.7016908093449,-4.06575814682064E-16));
#11942=CARTESIAN_POINT('',(6.67681390339618,6.7016908093449,-1.));
#11943=CARTESIAN_POINT('Origin',(6.67681390339618,6.7016908093449,-4.06575814682064E-16));
#11944=CARTESIAN_POINT('',(0.932251906823188,6.7016908093449,-1.));
#11945=CARTESIAN_POINT('',(26.,6.7016908093449,-1.));
#11946=CARTESIAN_POINT('',(0.932251906822564,6.70169080934177,1.));
#11947=CARTESIAN_POINT('Ctrl Pts',(0.932251906823183,6.70169080934491,-1.));
#11948=CARTESIAN_POINT('Ctrl Pts',(0.924248549049917,6.66131091017121,-1.));
#11949=CARTESIAN_POINT('Ctrl Pts',(0.916026356968957,6.62094102048031,-0.997554276745439));
#11950=CARTESIAN_POINT('Ctrl Pts',(0.881783128220109,6.45711744573232,-0.977603465009505));
#11951=CARTESIAN_POINT('Ctrl Pts',(0.854654659643743,6.33738348753352,-0.939561735078518));
#11952=CARTESIAN_POINT('Ctrl Pts',(0.800113400469254,6.11014608328131,-0.817261967795165));
#11953=CARTESIAN_POINT('Ctrl Pts',(0.77328444103289,6.00592553072582,-0.730775745996131));
#11954=CARTESIAN_POINT('Ctrl Pts',(0.729480326144063,5.8413149278795,-0.525593218279249));
#11955=CARTESIAN_POINT('Ctrl Pts',(0.712545126681715,5.78058813656252,-0.410370125980672));
#11956=CARTESIAN_POINT('Ctrl Pts',(0.694345193897906,5.71580700056676,-0.193362294484071));
#11957=CARTESIAN_POINT('Ctrl Pts',(0.690307391982312,5.70169080934487,-0.0970332031208705));
#11958=CARTESIAN_POINT('Ctrl Pts',(0.690307391982312,5.70169080934487,-5.70054262672731E-16));
#11959=CARTESIAN_POINT('Ctrl Pts',(0.690307391982312,5.70169080934487,0.126494091653897));
#11960=CARTESIAN_POINT('Ctrl Pts',(0.697192186740198,5.72567100919992,0.25144246077573));
#11961=CARTESIAN_POINT('Ctrl Pts',(0.723443573443553,5.81990229608856,0.48920911768999));
#11962=CARTESIAN_POINT('Ctrl Pts',(0.742874919145282,5.89055183127276,0.598815192100498));
#11963=CARTESIAN_POINT('Ctrl Pts',(0.787956450068906,6.06311917062026,0.779008106316694));
#11964=CARTESIAN_POINT('Ctrl Pts',(0.812798404624451,6.16166185353399,0.85019109475144));
#11965=CARTESIAN_POINT('Ctrl Pts',(0.864691942139612,6.38122379163014,0.955232747406083));
#11966=CARTESIAN_POINT('Ctrl Pts',(0.891412884359187,6.50130511642615,0.987456747739729));
#11967=CARTESIAN_POINT('Ctrl Pts',(0.921933001916271,6.65008201775339,0.999001452378396));
#11968=CARTESIAN_POINT('Ctrl Pts',(0.927138034517321,6.67588943272924,0.999999999999919));
#11969=CARTESIAN_POINT('Ctrl Pts',(0.93225190682257,6.70169080934177,1.));
#11970=CARTESIAN_POINT('Ctrl Pts',(0.93225190682257,6.70169080934177,1.));
#11971=CARTESIAN_POINT('Ctrl Pts',(0.95021663295712,6.7923294950717,1.00000000000028));
#11972=CARTESIAN_POINT('Ctrl Pts',(0.967037947810111,6.88289731649557,0.987678651235166));
#11973=CARTESIAN_POINT('Ctrl Pts',(1.00234665201365,7.08612514530952,0.930876070129687));
#11974=CARTESIAN_POINT('Ctrl Pts',(1.01939410567033,7.19503949676066,0.87813724044672));
#11975=CARTESIAN_POINT('Ctrl Pts',(1.04879439681428,7.39931145844304,0.728642051211854));
#11976=CARTESIAN_POINT('Ctrl Pts',(1.06022559732792,7.48994901935284,0.629606965290707));
#11977=CARTESIAN_POINT('Ctrl Pts',(1.07617030128948,7.62419484684745,0.406408985865648));
#11978=CARTESIAN_POINT('Ctrl Pts',(1.08086902511051,7.66842539636241,0.285763077415728));
#11979=CARTESIAN_POINT('Ctrl Pts',(1.0852457498272,7.70958096263185,0.0318261665609532));
#11980=CARTESIAN_POINT('Ctrl Pts',(1.08480714142453,7.70519119859556,-0.0991848216234942));
#11981=CARTESIAN_POINT('Ctrl Pts',(1.07843262498588,7.645938513344,-0.355002569322465));
#11982=CARTESIAN_POINT('Ctrl Pts',(1.07240914531565,7.59053680524487,-0.476976092322022));
#11983=CARTESIAN_POINT('Ctrl Pts',(1.05418970048312,7.44253010180747,-0.682447869986455));
#11984=CARTESIAN_POINT('Ctrl Pts',(1.04269942111853,7.35498368680039,-0.766583478682305));
#11985=CARTESIAN_POINT('Ctrl Pts',(1.0132565948215,7.15527406689819,-0.899197300474265));
#11986=CARTESIAN_POINT('Ctrl Pts',(0.995565232471033,7.0450187623199,-0.946689410696543));
#11987=CARTESIAN_POINT('Ctrl Pts',(0.961736774919552,6.85447725024748,-0.991251376980505));
#11988=CARTESIAN_POINT('Ctrl Pts',(0.947389466099236,6.7780653929409,-1.));
#11989=CARTESIAN_POINT('Ctrl Pts',(0.932251906823183,6.70169080934491,-1.));
#11990=CARTESIAN_POINT('Origin',(26.,6.7016908093449,-4.06575814682064E-16));
#11991=CARTESIAN_POINT('',(19.0677480931767,6.70169080934559,1.));
#11992=CARTESIAN_POINT('',(19.0677480931768,6.7016908093449,-1.));
#11993=CARTESIAN_POINT('Ctrl Pts',(19.0677480931765,6.70169080934669,1.));
#11994=CARTESIAN_POINT('Ctrl Pts',(19.0757514509498,6.6613109101724,1.00000000000007));
#11995=CARTESIAN_POINT('Ctrl Pts',(19.0839736430309,6.62094102048092,0.997554276745514));
#11996=CARTESIAN_POINT('Ctrl Pts',(19.1182168717799,6.45711744573232,0.977603465009509));
#11997=CARTESIAN_POINT('Ctrl Pts',(19.1453453403563,6.3373834875335,0.939561735078495));
#11998=CARTESIAN_POINT('Ctrl Pts',(19.1998865995307,6.11014608328137,0.817261967795189));
#11999=CARTESIAN_POINT('Ctrl Pts',(19.2267155589671,6.00592553072585,0.730775745996161));
#12000=CARTESIAN_POINT('Ctrl Pts',(19.2705196738559,5.84131492787951,0.525593218279265));
#12001=CARTESIAN_POINT('Ctrl Pts',(19.2874548733183,5.78058813656252,0.410370125980689));
#12002=CARTESIAN_POINT('Ctrl Pts',(19.3056548061021,5.71580700056676,0.193362294484076));
#12003=CARTESIAN_POINT('Ctrl Pts',(19.3096926080177,5.70169080934487,0.0970332031208726));
#12004=CARTESIAN_POINT('Ctrl Pts',(19.3096926080177,5.70169080934487,-5.70054262672731E-16));
#12005=CARTESIAN_POINT('Ctrl Pts',(19.3096926080177,5.70169080934487,-0.126494091653898));
#12006=CARTESIAN_POINT('Ctrl Pts',(19.3028078132598,5.72567100919992,-0.251442460775731));
#12007=CARTESIAN_POINT('Ctrl Pts',(19.2765564265564,5.81990229608856,-0.489209117689992));
#12008=CARTESIAN_POINT('Ctrl Pts',(19.2571250808547,5.89055183127276,-0.598815192100501));
#12009=CARTESIAN_POINT('Ctrl Pts',(19.2120435499311,6.06311917062025,-0.779008106316688));
#12010=CARTESIAN_POINT('Ctrl Pts',(19.1872015953756,6.16166185353397,-0.850191094751436));
#12011=CARTESIAN_POINT('Ctrl Pts',(19.1353080578604,6.38122379163016,-0.955232747406096));
#12012=CARTESIAN_POINT('Ctrl Pts',(19.1085871156408,6.50130511642616,-0.987456747739731));
#12013=CARTESIAN_POINT('Ctrl Pts',(19.0780669980835,6.65008201775443,-0.999001452378478));
#12014=CARTESIAN_POINT('Ctrl Pts',(19.0728619654823,6.67588943273133,-1.));
#12015=CARTESIAN_POINT('Ctrl Pts',(19.0677480931768,6.7016908093449,-1.));
#12016=CARTESIAN_POINT('',(13.7768139033962,6.7016908093449,-1.));
#12017=CARTESIAN_POINT('',(26.,6.7016908093449,-1.));
#12018=CARTESIAN_POINT('Origin',(13.7768139033962,6.7016908093449,-4.06575814682064E-16));
#12019=CARTESIAN_POINT('Ctrl Pts',(19.0677480931768,6.7016908093449,-1.));
#12020=CARTESIAN_POINT('Ctrl Pts',(19.0497833670425,6.79232949507379,-1.));
#12021=CARTESIAN_POINT('Ctrl Pts',(19.0329620521897,6.88289731649658,-0.987678651234883));
#12022=CARTESIAN_POINT('Ctrl Pts',(18.9976533479864,7.08612514530949,-0.930876070129694));
#12023=CARTESIAN_POINT('Ctrl Pts',(18.9806058943297,7.19503949676065,-0.878137240446731));
#12024=CARTESIAN_POINT('Ctrl Pts',(18.9512056031857,7.39931145844305,-0.728642051211849));
#12025=CARTESIAN_POINT('Ctrl Pts',(18.9397744026721,7.48994901935284,-0.629606965290706));
#12026=CARTESIAN_POINT('Ctrl Pts',(18.9238296987105,7.62419484684746,-0.40640898586564));
#12027=CARTESIAN_POINT('Ctrl Pts',(18.9191309748895,7.66842539636241,-0.285763077415725));
#12028=CARTESIAN_POINT('Ctrl Pts',(18.9147542501728,7.70958096263184,-0.0318261665609708));
#12029=CARTESIAN_POINT('Ctrl Pts',(18.9151928585755,7.70519119859557,0.0991848216234665));
#12030=CARTESIAN_POINT('Ctrl Pts',(18.9215673750141,7.64593851334401,0.355002569322444));
#12031=CARTESIAN_POINT('Ctrl Pts',(18.9275908546843,7.59053680524489,0.476976092321998));
#12032=CARTESIAN_POINT('Ctrl Pts',(18.9458102995169,7.44253010180748,0.682447869986442));
#12033=CARTESIAN_POINT('Ctrl Pts',(18.9573005788815,7.3549836868004,0.766583478682293));
#12034=CARTESIAN_POINT('Ctrl Pts',(18.9867434051785,7.1552740668982,0.89919730047426));
#12035=CARTESIAN_POINT('Ctrl Pts',(19.004434767529,7.0450187623199,0.946689410696536));
#12036=CARTESIAN_POINT('Ctrl Pts',(19.0382632250803,6.85447725024808,0.991251376980361));
#12037=CARTESIAN_POINT('Ctrl Pts',(19.0526105339005,6.77806539294211,0.999999999999863));
#12038=CARTESIAN_POINT('Ctrl Pts',(19.0677480931765,6.70169080934669,1.));
#12039=CARTESIAN_POINT('Ctrl Pts',(10.,22.6942090407623,-1.38777878078145E-16));
#12040=CARTESIAN_POINT('Ctrl Pts',(10.,22.6942090407623,-1.38777878078145E-16));
#12041=CARTESIAN_POINT('Ctrl Pts',(10.,22.6942090407623,0.));
#12042=CARTESIAN_POINT('Ctrl Pts',(10.,22.6942090407623,1.38777878078145E-16));
#12043=CARTESIAN_POINT('Ctrl Pts',(10.,22.6942090407623,1.38777878078145E-16));
#12044=CARTESIAN_POINT('Ctrl Pts',(10.,22.6942090407623,1.38777878078145E-16));
#12045=CARTESIAN_POINT('Ctrl Pts',(10.,22.6942090407623,0.));
#12046=CARTESIAN_POINT('Ctrl Pts',(10.,22.6942090407623,-1.38777878078145E-16));
#12047=CARTESIAN_POINT('Ctrl Pts',(10.,22.6942090407623,-1.38777878078145E-16));
#12048=CARTESIAN_POINT('Ctrl Pts',(10.,22.9763860067717,3.03546549996621));
#12049=CARTESIAN_POINT('Ctrl Pts',(6.96453450003379,22.9763860067717,3.03546549996621));
#12050=CARTESIAN_POINT('Ctrl Pts',(6.96453450003379,22.9763860067717,0.));
#12051=CARTESIAN_POINT('Ctrl Pts',(6.96453450003379,22.9763860067717,-3.03546549996621));
#12052=CARTESIAN_POINT('Ctrl Pts',(10.,22.9763860067717,-3.03546549996621));
#12053=CARTESIAN_POINT('Ctrl Pts',(13.0354654999662,22.9763860067717,-3.03546549996621));
#12054=CARTESIAN_POINT('Ctrl Pts',(13.0354654999662,22.9763860067717,0.));
#12055=CARTESIAN_POINT('Ctrl Pts',(13.0354654999662,22.9763860067717,3.03546549996621));
#12056=CARTESIAN_POINT('Ctrl Pts',(10.,22.9763860067717,3.03546549996621));
#12057=CARTESIAN_POINT('Ctrl Pts',(10.,20.2758418106305,4.44993914281691));
#12058=CARTESIAN_POINT('Ctrl Pts',(5.55006085718309,20.2758418106305,4.44993914281691));
#12059=CARTESIAN_POINT('Ctrl Pts',(5.55006085718309,20.2758418106305,0.));
#12060=CARTESIAN_POINT('Ctrl Pts',(5.55006085718309,20.2758418106305,-4.44993914281691));
#12061=CARTESIAN_POINT('Ctrl Pts',(10.,20.2758418106305,-4.44993914281691));
#12062=CARTESIAN_POINT('Ctrl Pts',(14.4499391428169,20.2758418106305,-4.44993914281691));
#12063=CARTESIAN_POINT('Ctrl Pts',(14.4499391428169,20.2758418106305,0.));
#12064=CARTESIAN_POINT('Ctrl Pts',(14.4499391428169,20.2758418106305,4.44993914281691));
#12065=CARTESIAN_POINT('Ctrl Pts',(10.,20.2758418106305,4.44993914281691));
#12066=CARTESIAN_POINT('',(10.,20.2758418106305,4.44993914281691));
#12067=CARTESIAN_POINT('Origin',(10.,20.2758418106305,0.));
#12068=CARTESIAN_POINT('',(10.,22.6942090407623,0.));
#12069=CARTESIAN_POINT('Origin',(10.,18.165580311944,0.420981465576021));
#12070=CARTESIAN_POINT('Ctrl Pts',(10.,20.2758418106305,4.44993914281691));
#12071=CARTESIAN_POINT('Ctrl Pts',(5.5500608571831,20.2758418106305,4.4499391428169));
#12072=CARTESIAN_POINT('Ctrl Pts',(5.5500608571831,20.2758418106305,0.));
#12073=CARTESIAN_POINT('Ctrl Pts',(5.5500608571831,20.2758418106305,-4.4499391428169));
#12074=CARTESIAN_POINT('Ctrl Pts',(10.,20.2758418106305,-4.44993914281691));
#12075=CARTESIAN_POINT('Ctrl Pts',(14.4499391428169,20.2758418106305,-4.4499391428169));
#12076=CARTESIAN_POINT('Ctrl Pts',(14.4499391428169,20.2758418106305,0.));
#12077=CARTESIAN_POINT('Ctrl Pts',(14.4499391428169,20.2758418106305,4.4499391428169));
#12078=CARTESIAN_POINT('Ctrl Pts',(10.,20.2758418106305,4.44993914281691));
#12079=CARTESIAN_POINT('Ctrl Pts',(10.,10.6889014672656,9.30235729258629));
#12080=CARTESIAN_POINT('Ctrl Pts',(0.697642707413711,10.6889014672656,9.30235729258629));
#12081=CARTESIAN_POINT('Ctrl Pts',(0.697642707413709,10.6889014672656,0.));
#12082=CARTESIAN_POINT('Ctrl Pts',(0.697642707413711,10.6889014672656,-9.30235729258629));
#12083=CARTESIAN_POINT('Ctrl Pts',(10.,10.6889014672656,-9.30235729258629));
#12084=CARTESIAN_POINT('Ctrl Pts',(19.3023572925863,10.6889014672656,-9.30235729258629));
#12085=CARTESIAN_POINT('Ctrl Pts',(19.3023572925863,10.6889014672656,0.));
#12086=CARTESIAN_POINT('Ctrl Pts',(19.3023572925863,10.6889014672656,9.30235729258629));
#12087=CARTESIAN_POINT('Ctrl Pts',(10.,10.6889014672656,9.30235729258629));
#12088=CARTESIAN_POINT('Ctrl Pts',(10.,-0.0333011709430475,10.0021841516323));
#12089=CARTESIAN_POINT('Ctrl Pts',(-0.00218415163227181,-0.0333011709430475,
10.0021841516323));
#12090=CARTESIAN_POINT('Ctrl Pts',(-0.00218415163227403,-0.0333011709430475,
0.));
#12091=CARTESIAN_POINT('Ctrl Pts',(-0.00218415163227181,-0.0333011709430475,
-10.0021841516323));
#12092=CARTESIAN_POINT('Ctrl Pts',(10.,-0.0333011709430475,-10.0021841516323));
#12093=CARTESIAN_POINT('Ctrl Pts',(20.0021841516323,-0.0333011709430475,
-10.0021841516323));
#12094=CARTESIAN_POINT('Ctrl Pts',(20.0021841516323,-0.0333011709430475,
0.));
#12095=CARTESIAN_POINT('Ctrl Pts',(20.0021841516323,-0.0333011709430475,
10.0021841516323));
#12096=CARTESIAN_POINT('Ctrl Pts',(10.,-0.0333011709430475,10.0021841516323));
#12097=CARTESIAN_POINT('',(9.99999987317287,0.000194077067732489,10.0000928969774));
#12098=CARTESIAN_POINT('Ctrl Pts',(9.99999987317287,0.000194077067732486,
10.0000928969774));
#12099=CARTESIAN_POINT('Ctrl Pts',(9.80810904601693,9.1950696030043E-5,
10.0000442778392));
#12100=CARTESIAN_POINT('Ctrl Pts',(9.61573304980258,0.00331798875440397,
9.99425980218522));
#12101=CARTESIAN_POINT('Ctrl Pts',(8.33291717935469,0.0477168426728619,
9.91718091357786));
#12102=CARTESIAN_POINT('Ctrl Pts',(7.27724454850721,0.193447639956633,9.66841352790813));
#12103=CARTESIAN_POINT('Ctrl Pts',(5.18973500313614,0.649166839307786,8.79546486797327));
#12104=CARTESIAN_POINT('Ctrl Pts',(4.19507286136815,0.969114760287138,8.13936989246473));
#12105=CARTESIAN_POINT('Ctrl Pts',(2.40058556231555,1.64336913807273,6.42724037761097));
#12106=CARTESIAN_POINT('Ctrl Pts',(1.63759314204628,1.99433660295155,5.33756391116479));
#12107=CARTESIAN_POINT('Ctrl Pts',(0.823620674034291,2.38573688258387,3.47744015908405));
#12108=CARTESIAN_POINT('Ctrl Pts',(0.608585489527882,2.49400970267041,2.8055797921226));
#12109=CARTESIAN_POINT('Ctrl Pts',(0.3189262235327,2.64124370193303,1.41915458981438));
#12110=CARTESIAN_POINT('Ctrl Pts',(0.245631819034601,2.67949192431123,0.711701241816013));
#12111=CARTESIAN_POINT('Ctrl Pts',(0.2456318190346,2.67949192431123,5.96744875736022E-15));
#12112=CARTESIAN_POINT('Ctrl Pts',(0.245631819034601,2.67949192431123,-1.20289765945603));
#12113=CARTESIAN_POINT('Ctrl Pts',(0.454406269039078,2.56890479083654,-2.3863380426886));
#12114=CARTESIAN_POINT('Ctrl Pts',(1.28433866991227,2.16096119478927,-4.68032816011342));
#12115=CARTESIAN_POINT('Ctrl Pts',(1.91916845937342,1.85829341673215,-5.75624332867574));
#12116=CARTESIAN_POINT('Ctrl Pts',(3.59440265680175,1.17782954694983,-7.67651894426489));
#12117=CARTESIAN_POINT('Ctrl Pts',(4.65794493564582,0.799305541817284,-8.49042605227953));
#12118=CARTESIAN_POINT('Ctrl Pts',(6.89944797346244,0.256191889285011,-9.55859137985788));
#12119=CARTESIAN_POINT('Ctrl Pts',(8.02464547197843,0.0758487766023874,
-9.86811069108096));
#12120=CARTESIAN_POINT('Ctrl Pts',(10.2891271125017,-0.033299425832443,
-10.0580114046642));
#12121=CARTESIAN_POINT('Ctrl Pts',(11.3784610421618,0.0243895637395715,
-9.96258304339045));
#12122=CARTESIAN_POINT('Ctrl Pts',(13.5297527353772,0.335468227226224,-9.40075939411568));
#12123=CARTESIAN_POINT('Ctrl Pts',(14.5547382087638,0.591005341871764,-8.92516032239902));
#12124=CARTESIAN_POINT('Ctrl Pts',(16.516698088114,1.20843453126161,-7.57040193616715));
#12125=CARTESIAN_POINT('Ctrl Pts',(17.4122595410463,1.57578375247122,-6.64681501561899));
#12126=CARTESIAN_POINT('Ctrl Pts',(18.8002236181422,2.1943040052823,-4.51505601963387));
#12127=CARTESIAN_POINT('Ctrl Pts',(19.2902956110326,2.44248890127282,-3.32400070588094));
#12128=CARTESIAN_POINT('Ctrl Pts',(19.7901343922786,2.696799472177,-0.863253693613933));
#12129=CARTESIAN_POINT('Ctrl Pts',(19.8198403086391,2.71274440835119,0.36216566135821));
#12130=CARTESIAN_POINT('Ctrl Pts',(19.450604566805,2.52354005493898,2.7684762978899));
#12131=CARTESIAN_POINT('Ctrl Pts',(19.0587240926145,2.322406562892,3.91259636003955));
#12132=CARTESIAN_POINT('Ctrl Pts',(17.8594783884844,1.76766583827933,6.08297459859969));
#12133=CARTESIAN_POINT('Ctrl Pts',(17.0268766086191,1.40663102240569,7.07457363856991));
#12134=CARTESIAN_POINT('Ctrl Pts',(15.0677936986477,0.732379395365387,8.64898495762566));
#12135=CARTESIAN_POINT('Ctrl Pts',(13.9536542495791,0.421460567512847,9.24076616447532));
#12136=CARTESIAN_POINT('Ctrl Pts',(11.8519809404125,0.0796474466335174,
9.86534193353201));
#12137=CARTESIAN_POINT('Ctrl Pts',(10.9317093488347,0.000689942918333018,
10.0003289630384));
#12138=CARTESIAN_POINT('Ctrl Pts',(9.99999987317287,0.000194077067732486,
10.0000928969774));
#12139=CARTESIAN_POINT('Ctrl Pts',(10.,0.000187141247131616,9.99998766579631));
#12140=CARTESIAN_POINT('Ctrl Pts',(10.,10.7044979812508,9.29446313607499));
#12141=CARTESIAN_POINT('Ctrl Pts',(10.,20.2758418106305,4.44993914281691));
#12142=CARTESIAN_POINT('Origin',(24.,-17.3205080756888,4.50694379621148E-15));
#12143=CARTESIAN_POINT('',(13.7768139033962,1.77236952303898,5.955));
#12144=CARTESIAN_POINT('',(13.7768139033962,1.77236952303898,-5.955));
#12145=CARTESIAN_POINT('Origin',(13.7768139033962,-17.3205080756888,4.50694379621148E-15));
#12146=CARTESIAN_POINT('',(6.67681390339618,1.77236952303898,-5.955));
#12147=CARTESIAN_POINT('',(24.,1.77236952303898,-5.955));
#12148=CARTESIAN_POINT('',(6.67681390339617,1.77236952303898,5.955));
#12149=CARTESIAN_POINT('Origin',(6.67681390339618,-17.3205080756888,4.50694379621148E-15));
#12150=CARTESIAN_POINT('',(24.,1.77236952303898,5.955));
#12151=CARTESIAN_POINT('Origin',(0.,10.,0.));
#12152=CARTESIAN_POINT('',(13.7768139033962,10.,-5.955));
#12153=CARTESIAN_POINT('',(13.7768139033962,10.,5.955));
#12154=CARTESIAN_POINT('',(13.7768139033962,10.,5.955));
#12155=CARTESIAN_POINT('',(6.67681390339617,10.,5.955));
#12156=CARTESIAN_POINT('',(6.67681390339617,10.,5.955));
#12157=CARTESIAN_POINT('',(6.67681390339618,10.,-5.955));
#12158=CARTESIAN_POINT('',(6.67681390339617,10.,5.955));
#12159=CARTESIAN_POINT('',(6.67681390339618,10.,-5.955));
#12160=CARTESIAN_POINT('Origin',(6.67681390339617,10.,5.955));
#12161=CARTESIAN_POINT('',(6.67681390339617,10.,5.955));
#12162=CARTESIAN_POINT('',(13.7768139033962,10.,5.955));
#12163=CARTESIAN_POINT('Origin',(6.67681390339617,10.,5.955));
#12164=CARTESIAN_POINT('',(6.67681390339618,10.,-5.955));
#12165=CARTESIAN_POINT('Origin',(6.67681390339618,10.,-5.955));
#12166=CARTESIAN_POINT('',(13.7768139033962,10.,-5.955));
#12167=CARTESIAN_POINT('Origin',(13.7768139033962,10.,5.955));
#12168=CARTESIAN_POINT('',(1.94208271978831,2.32007362280668,28.6270964283021));
#12169=CARTESIAN_POINT('',(-5.63914822227041,2.32007241709248,61.9072863102119));
#12170=CARTESIAN_POINT('',(10.0018112394065,2.32007121137827,91.770525425635));
#12171=CARTESIAN_POINT('',(-14.0216357734545,-9.80481262358417,32.06283057294));
#12172=CARTESIAN_POINT('',(-11.1720018984223,-11.6348126235842,76.3089841024205));
#12173=CARTESIAN_POINT('',(28.7814411963245,3.57687209243893,-23.5152842220037));
#12174=CARTESIAN_POINT('',(39.8404107172023,12.5468875262028,86.121686806841));
#12175=CARTESIAN_POINT('',(0.,0.,0.));
#12176=CARTESIAN_POINT('',(0.,0.,0.));
#12177=CARTESIAN_POINT('Origin',(0.,40.8397926572471,-1.59119787916534));
#12178=CARTESIAN_POINT('',(-1.22464679914735E-16,39.3677205542196,9.23045840289062));
#12179=CARTESIAN_POINT('Origin',(0.,38.3933504894344,9.00550734854675));
#12180=CARTESIAN_POINT('',(-1.22464679914735E-16,41.1779050581859,1.3896878959578));
#12181=CARTESIAN_POINT('',(-1.22464679914735E-16,41.8141627220323,-1.36624682482147));
#12182=CARTESIAN_POINT('Origin',(0.,40.2035349934007,1.16473684161393));
#12183=CARTESIAN_POINT('Origin',(-20.6306248908449,20.2436822747633,-12.1953723836195));
#12184=CARTESIAN_POINT('',(-20.6306248908449,20.5804821002219,-6.98609547817754));
#12185=CARTESIAN_POINT('Origin',(-20.6306248908449,19.118927003044,-7.32352205969334));
#12186=CARTESIAN_POINT('',(-20.6306248908449,17.2062162850639,7.629455493601));
#12187=CARTESIAN_POINT('',(-20.6306248908449,21.7052373719412,-11.8579458021037));
#12188=CARTESIAN_POINT('Origin',(-20.6306248908449,15.744661187886,7.29202891208519));
#12189=CARTESIAN_POINT('Origin',(0.,17.5,19.325));
#12190=CARTESIAN_POINT('',(1.5,17.5,-3.675));
#12191=CARTESIAN_POINT('Origin',(0.,17.5,-3.675));
#12192=CARTESIAN_POINT('',(1.5,17.5,-17.4355957741627));
#12193=CARTESIAN_POINT('',(1.5,17.5,19.325));
#12194=CARTESIAN_POINT('Origin',(0.,17.5,-17.4355957741627));
#12195=CARTESIAN_POINT('Origin',(0.,17.5,19.325));
#12196=CARTESIAN_POINT('',(1.5,17.5,17.4355957741627));
#12197=CARTESIAN_POINT('Origin',(0.,17.5,17.4355957741627));
#12198=CARTESIAN_POINT('',(1.5,17.5,3.675));
#12199=CARTESIAN_POINT('',(1.5,17.5,19.325));
#12200=CARTESIAN_POINT('Origin',(0.,17.5,3.675));
#12201=CARTESIAN_POINT('Origin',(0.,17.5,0.));
#12202=CARTESIAN_POINT('',(17.1097742533325,17.5,-3.675));
#12203=CARTESIAN_POINT('Origin',(0.,17.5,0.));
#12204=CARTESIAN_POINT('',(-16.,11.4382861334438,-3.675));
#12205=CARTESIAN_POINT('Origin',(0.,17.5,-3.675));
#12206=CARTESIAN_POINT('',(-16.,11.4382861334438,3.675));
#12207=CARTESIAN_POINT('Origin',(-16.,17.5,0.));
#12208=CARTESIAN_POINT('',(17.1097742533325,17.5,3.675));
#12209=CARTESIAN_POINT('Origin',(0.,17.5,3.675));
#12210=CARTESIAN_POINT('Origin',(0.,17.5,0.));
#12211=CARTESIAN_POINT('',(16.5215428428775,21.9478081220939,3.675));
#12212=CARTESIAN_POINT('Origin',(0.,17.5,3.675));
#12213=CARTESIAN_POINT('',(16.5215428428775,21.9478081220939,-3.675));
#12214=CARTESIAN_POINT('Origin',(0.,21.9478081220939,0.));
#12215=CARTESIAN_POINT('Origin',(0.,17.5,-3.675));
#12216=CARTESIAN_POINT('',(-2.14861257031475,34.7331056821866,-2.15720480466577));
#12217=CARTESIAN_POINT('',(-2.14861257031475,32.0433564423134,9.49337913571913));
#12218=CARTESIAN_POINT('Origin',(-2.14861257031475,17.5,0.));
#12219=CARTESIAN_POINT('',(2.14861257031475,34.7331056821866,-2.15720480466577));
#12220=CARTESIAN_POINT('Origin',(0.,18.8448746199366,-5.82529197019245));
#12221=CARTESIAN_POINT('',(2.14861257031475,32.0433564423134,9.49337913571913));
#12222=CARTESIAN_POINT('Origin',(2.14861257031475,17.5,0.));
#12223=CARTESIAN_POINT('Origin',(0.,16.1551253800634,5.82529197019245));
#12224=CARTESIAN_POINT('',(-15.2970585407784,23.08461316672,-6.4079712685138));
#12225=CARTESIAN_POINT('',(-15.2970585407784,19.7103473515619,8.20757970326472));
#12226=CARTESIAN_POINT('Origin',(0.,21.3974802591409,0.899804217375471));
#12227=CARTESIAN_POINT('',(-15.2970585407784,11.9153868332801,6.4079712685138));
#12228=CARTESIAN_POINT('Origin',(0.,15.812867092421,7.30777548588927));
#12229=CARTESIAN_POINT('',(-15.2970585407784,15.2896526484381,-8.20757970326472));
#12230=CARTESIAN_POINT('Origin',(0.,13.6025197408591,-0.89980421737547));
#12231=CARTESIAN_POINT('Origin',(0.,19.187132907579,-7.30777548588926));
#12232=CARTESIAN_POINT('Origin',(0.,39.9993294599633,9.2345728386573));
#12233=CARTESIAN_POINT('',(-2.14861257031475,39.9682699940902,9.369106165755));
#12234=CARTESIAN_POINT('',(2.14861257031475,39.9682699940902,9.369106165755));
#12235=CARTESIAN_POINT('',(0.,39.9682699940902,9.369106165755));
#12236=CARTESIAN_POINT('',(-2.14861257031475,39.540006934909,11.2241172744453));
#12237=CARTESIAN_POINT('',(-2.14861257031475,42.2297561747823,-0.426466665939627));
#12238=CARTESIAN_POINT('',(2.14861257031475,39.540006934909,11.2241172744453));
#12239=CARTESIAN_POINT('',(-2.14861257031475,39.540006934909,11.2241172744453));
#12240=CARTESIAN_POINT('',(2.14861257031475,42.2297561747823,-0.426466665939627));
#12241=CARTESIAN_POINT('Origin',(-23.,20.5119281642586,4.73555175177994));
#12242=CARTESIAN_POINT('',(-23.,23.08461316672,-6.4079712685138));
#12243=CARTESIAN_POINT('',(-23.,23.08461316672,-6.4079712685138));
#12244=CARTESIAN_POINT('',(-23.,19.7103473515619,8.20757970326472));
#12245=CARTESIAN_POINT('',(-23.,20.5119281642586,4.73555175177994));
#12246=CARTESIAN_POINT('',(-23.,19.7103473515619,8.20757970326472));
#12247=CARTESIAN_POINT('Origin',(-23.,2.57268500246128,-11.1435230202937));
#12248=CARTESIAN_POINT('',(-23.,15.2896526484381,-8.20757970326472));
#12249=CARTESIAN_POINT('',(-23.,15.2896526484381,-8.20757970326472));
#12250=CARTESIAN_POINT('',(-23.,2.57268500246128,-11.1435230202937));
#12251=CARTESIAN_POINT('Origin',(-23.,12.7169676459768,2.935943317029));
#12252=CARTESIAN_POINT('',(-23.,11.9153868332801,6.4079712685138));
#12253=CARTESIAN_POINT('',(-23.,11.9153868332801,6.4079712685138));
#12254=CARTESIAN_POINT('',(-23.,12.7169676459768,2.935943317029));
#12255=CARTESIAN_POINT('Origin',(-23.,-0.801580812696699,3.47202795148484));
#12256=CARTESIAN_POINT('',(-23.,-0.801580812696699,3.47202795148484));
#12257=CARTESIAN_POINT('Origin',(-23.,0.,0.));
#12258=CARTESIAN_POINT('Origin',(25.,21.9478081220939,-3.675));
#12259=CARTESIAN_POINT('',(-16.,21.9478081220939,-3.675));
#12260=CARTESIAN_POINT('',(25.,21.9478081220939,-3.675));
#12261=CARTESIAN_POINT('',(-16.,21.9478081220939,-3.675));
#12262=CARTESIAN_POINT('Origin',(25.,21.9478081220939,3.675));
#12263=CARTESIAN_POINT('',(-16.,21.9478081220939,3.675));
#12264=CARTESIAN_POINT('',(25.,21.9478081220939,3.675));
#12265=CARTESIAN_POINT('',(-16.,21.9478081220939,3.675));
#12266=CARTESIAN_POINT('Origin',(25.,21.9478081220939,3.675));
#12267=CARTESIAN_POINT('',(-16.,21.9478081220939,3.675));
#12268=CARTESIAN_POINT('Origin',(-16.,0.,0.));
#12269=CARTESIAN_POINT('Origin',(2.14861257031475,42.2297561747823,-0.426466665939627));
#12270=CARTESIAN_POINT('',(2.14861257031475,37.1837280639145,0.467559478255006));
#12271=CARTESIAN_POINT('',(2.14861257031475,35.3735435599482,8.30832998518782));
#12272=CARTESIAN_POINT('',(2.14861257031475,37.6350297406403,-1.4872428465068));
#12273=CARTESIAN_POINT('',(2.14861257031475,39.9682699940902,9.369106165755));
#12274=CARTESIAN_POINT('',(2.14861257031475,39.540006934909,11.2241172744453));
#12275=CARTESIAN_POINT('',(2.14861257031475,42.2297561747823,-0.426466665939627));
#12276=CARTESIAN_POINT('',(2.14861257031475,42.2297561747823,-0.426466665939627));
#12277=CARTESIAN_POINT('',(2.14861257031475,41.7784544980564,1.52833565882218));
#12278=CARTESIAN_POINT('',(2.14861257031475,42.2297561747823,-0.426466665939627));
#12279=CARTESIAN_POINT('',(2.14861257031475,41.7784544980564,1.52833565882218));
#12280=CARTESIAN_POINT('Origin',(-2.14861257031475,42.2297561747823,-0.426466665939627));
#12281=CARTESIAN_POINT('',(-2.14861257031475,42.2297561747823,-0.426466665939627));
#12282=CARTESIAN_POINT('',(-2.14861257031475,42.2297561747823,-0.426466665939627));
#12283=CARTESIAN_POINT('',(-2.14861257031475,42.2297561747823,-0.426466665939627));
#12284=CARTESIAN_POINT('Origin',(-2.14861257031475,42.2297561747823,-0.426466665939627));
#12285=CARTESIAN_POINT('',(-2.14861257031475,35.3735435599482,8.30832998518782));
#12286=CARTESIAN_POINT('',(-2.14861257031475,35.3735435599482,8.30832998518782));
#12287=CARTESIAN_POINT('',(-2.14861257031475,37.1837280639145,0.467559478255006));
#12288=CARTESIAN_POINT('',(-2.14861257031475,37.1837280639145,0.467559478255006));
#12289=CARTESIAN_POINT('',(-2.14861257031475,41.7784544980564,1.52833565882219));
#12290=CARTESIAN_POINT('',(-2.14861257031475,41.7784544980564,1.52833565882219));
#12291=CARTESIAN_POINT('',(-2.14861257031475,42.2297561747823,-0.426466665939627));
#12292=CARTESIAN_POINT('',(-2.14861257031475,39.540006934909,11.2241172744453));
#12293=CARTESIAN_POINT('Origin',(-2.14861257031475,39.540006934909,11.2241172744453));
#12294=CARTESIAN_POINT('Origin',(0.,39.9993294599633,9.2345728386573));
#12295=CARTESIAN_POINT('',(0.,41.7784544980564,1.52833565882218));
#12296=CARTESIAN_POINT('Origin',(7.85138742968525,37.1837280639145,0.467559478255006));
#12297=CARTESIAN_POINT('',(7.85138742968525,37.1837280639145,0.467559478255006));
#12298=CARTESIAN_POINT('',(7.85138742968525,35.3735435599482,8.30832998518782));
#12299=CARTESIAN_POINT('Origin',(7.85138742968525,35.3735435599482,8.30832998518782));
#12300=CARTESIAN_POINT('Origin',(7.85138742968525,41.7784544980564,1.52833565882219));
#12301=CARTESIAN_POINT('',(0.,0.,0.));
#12302=CARTESIAN_POINT('Origin',(0.095196568285859,-18.,33.232185266773));
#12303=CARTESIAN_POINT('',(0.0951965682858588,-7.5,31.732185266773));
#12304=CARTESIAN_POINT('Origin',(0.095196568285859,-7.5,33.232185266773));
#12305=CARTESIAN_POINT('',(0.0951965682858588,7.5,31.732185266773));
#12306=CARTESIAN_POINT('',(0.0951965682858588,-18.,31.732185266773));
#12307=CARTESIAN_POINT('Origin',(0.095196568285859,7.5,33.232185266773));
#12308=CARTESIAN_POINT('Origin',(0.0951965682858563,19.8000040922037,8.14863870441721));
#12309=CARTESIAN_POINT('',(0.0951965682858561,-8.24999590779632,9.79863870441721));
#12310=CARTESIAN_POINT('Origin',(0.0951965682858563,-8.24999590779632,8.14863870441721));
#12311=CARTESIAN_POINT('',(0.0951965682858558,-14.0999162292878,9.79863870441721));
#12312=CARTESIAN_POINT('',(0.0951965682858561,19.8000040922037,9.79863870441721));
#12313=CARTESIAN_POINT('',(0.0951965682858563,-14.1575179435509,6.49863870441721));
#12314=CARTESIAN_POINT('Ctrl Pts',(0.0951965682858559,-14.0999162292878,
9.79863870441721));
#12315=CARTESIAN_POINT('Ctrl Pts',(-0.111884389331936,-14.0999162292878,
9.79863870441721));
#12316=CARTESIAN_POINT('Ctrl Pts',(-0.332690322215915,-14.0956093061338,
9.7572743886747));
#12317=CARTESIAN_POINT('Ctrl Pts',(-0.738813012790702,-14.0803572376207,
9.58920247165813));
#12318=CARTESIAN_POINT('Ctrl Pts',(-0.9241426028172,-14.0696692652477,9.46250263892422));
#12319=CARTESIAN_POINT('Ctrl Pts',(-1.21685503126047,-14.0505183636864,
9.17028693794665));
#12320=CARTESIAN_POINT('Ctrl Pts',(-1.34384871039232,-14.0408156535701,
8.98524545523767));
#12321=CARTESIAN_POINT('Ctrl Pts',(-1.5126138598668,-14.0296199070515,8.57957694362764));
#12322=CARTESIAN_POINT('Ctrl Pts',(-1.55437816863629,-14.0283939252263,
8.35893960919315));
#12323=CARTESIAN_POINT('Ctrl Pts',(-1.55522352628415,-14.0355830590593,
7.94423675389232));
#12324=CARTESIAN_POINT('Ctrl Pts',(-1.51404500481727,-14.0445114051257,
7.72278149953618));
#12325=CARTESIAN_POINT('Ctrl Pts',(-1.34599446823065,-14.0698943839908,
7.31558332529204));
#12326=CARTESIAN_POINT('Ctrl Pts',(-1.21913545885449,-14.0860803724786,
7.12981833652177));
#12327=CARTESIAN_POINT('Ctrl Pts',(-0.926341065508513,-14.1154701420388,
6.83642648344605));
#12328=CARTESIAN_POINT('Ctrl Pts',(-0.740831328663387,-14.1305991784691,
6.70916694867708));
#12329=CARTESIAN_POINT('Ctrl Pts',(-0.33394200376843,-14.1517518463386,
6.54026633590998));
#12330=CARTESIAN_POINT('Ctrl Pts',(-0.112543486877898,-14.1575179435509,
6.49863870441721));
#12331=CARTESIAN_POINT('Ctrl Pts',(0.0951965682858563,-14.1575179435509,
6.49863870441721));
#12332=CARTESIAN_POINT('Ctrl Pts',(0.0951965682858563,-14.1575179435509,
6.49863870441721));
#12333=CARTESIAN_POINT('Ctrl Pts',(0.302936623449611,-14.1575179435509,
6.49863870441721));
#12334=CARTESIAN_POINT('Ctrl Pts',(0.524335140340142,-14.1517518463386,
6.54026633590998));
#12335=CARTESIAN_POINT('Ctrl Pts',(0.931224465235098,-14.1305991784691,
6.70916694867708));
#12336=CARTESIAN_POINT('Ctrl Pts',(1.11673420208023,-14.1154701420388,6.83642648344605));
#12337=CARTESIAN_POINT('Ctrl Pts',(1.4095285954262,-14.0860803724786,7.12981833652177));
#12338=CARTESIAN_POINT('Ctrl Pts',(1.53638760480237,-14.0698943839908,7.31558332529205));
#12339=CARTESIAN_POINT('Ctrl Pts',(1.70443814138898,-14.0445114051257,7.72278149953618));
#12340=CARTESIAN_POINT('Ctrl Pts',(1.74561666285586,-14.0355830590593,7.94423675389232));
#12341=CARTESIAN_POINT('Ctrl Pts',(1.74519314013823,-14.0319813154587,8.15200216623844));
#12342=CARTESIAN_POINT('Ctrl Pts',(1.744771305208,-14.0283939252263,8.35893960919316));
#12343=CARTESIAN_POINT('Ctrl Pts',(1.70300699643852,-14.0296199070515,8.57957694362764));
#12344=CARTESIAN_POINT('Ctrl Pts',(1.53424184696403,-14.0408156535701,8.98524545523767));
#12345=CARTESIAN_POINT('Ctrl Pts',(1.40724816783219,-14.0505183636864,9.17028693794665));
#12346=CARTESIAN_POINT('Ctrl Pts',(1.11453573938891,-14.0696692652477,9.46250263892422));
#12347=CARTESIAN_POINT('Ctrl Pts',(0.929206149362414,-14.0803572376207,
9.58920247165813));
#12348=CARTESIAN_POINT('Ctrl Pts',(0.523083458787627,-14.0956093061338,
9.7572743886747));
#12349=CARTESIAN_POINT('Ctrl Pts',(0.302277525903648,-14.0999162292878,
9.79863870441721));
#12350=CARTESIAN_POINT('Ctrl Pts',(0.095196568285856,-14.0999162292878,
9.79863870441721));
#12351=CARTESIAN_POINT('Origin',(0.0951965682858563,19.8000040922037,8.14863870441721));
#12352=CARTESIAN_POINT('',(0.0951965682865928,14.1575261279592,6.49863870441022));
#12353=CARTESIAN_POINT('',(0.0951965682858563,14.0999244136952,9.79863870441721));
#12354=CARTESIAN_POINT('Ctrl Pts',(0.0951965682858558,14.1575261279583,
6.49863870441721));
#12355=CARTESIAN_POINT('Ctrl Pts',(-0.112543486877899,14.1575261279583,
6.49863870441721));
#12356=CARTESIAN_POINT('Ctrl Pts',(-0.33394200376843,14.151760030746,6.54026633590998));
#12357=CARTESIAN_POINT('Ctrl Pts',(-0.740831328663387,14.1306073628765,
6.70916694867708));
#12358=CARTESIAN_POINT('Ctrl Pts',(-0.926341065508513,14.1154783264462,
6.83642648344605));
#12359=CARTESIAN_POINT('Ctrl Pts',(-1.21913545885449,14.0860885568859,7.12981833652177));
#12360=CARTESIAN_POINT('Ctrl Pts',(-1.34599446823065,14.0699025683982,7.31558332529205));
#12361=CARTESIAN_POINT('Ctrl Pts',(-1.51404500481727,14.0445195895331,7.72278149953618));
#12362=CARTESIAN_POINT('Ctrl Pts',(-1.55522352628415,14.0355912434667,7.94423675389232));
#12363=CARTESIAN_POINT('Ctrl Pts',(-1.55437816863629,14.0284021096337,8.35893960919315));
#12364=CARTESIAN_POINT('Ctrl Pts',(-1.5126138598668,14.0296280914589,8.57957694362764));
#12365=CARTESIAN_POINT('Ctrl Pts',(-1.34384871039232,14.0408238379775,8.98524545523767));
#12366=CARTESIAN_POINT('Ctrl Pts',(-1.21685503126047,14.0505265480937,9.17028693794665));
#12367=CARTESIAN_POINT('Ctrl Pts',(-0.9241426028172,14.0696774496551,9.46250263892422));
#12368=CARTESIAN_POINT('Ctrl Pts',(-0.738813012790702,14.080365422028,9.58920247165813));
#12369=CARTESIAN_POINT('Ctrl Pts',(-0.332690322215915,14.0956174905411,
9.7572743886747));
#12370=CARTESIAN_POINT('Ctrl Pts',(-0.111884389331936,14.0999244136952,
9.79863870441721));
#12371=CARTESIAN_POINT('Ctrl Pts',(0.0951965682858565,14.0999244136952,
9.79863870441721));
#12372=CARTESIAN_POINT('',(0.0951965682858561,8.25000409220368,9.79863870441721));
#12373=CARTESIAN_POINT('',(0.0951965682858561,19.8000040922037,9.79863870441721));
#12374=CARTESIAN_POINT('Origin',(0.0951965682858563,8.25000409220368,8.14863870441721));
#12375=CARTESIAN_POINT('Ctrl Pts',(0.0951965682858564,14.0999244136952,
9.79863870441721));
#12376=CARTESIAN_POINT('Ctrl Pts',(0.302277525903648,14.0999244136952,9.79863870441721));
#12377=CARTESIAN_POINT('Ctrl Pts',(0.523083458787627,14.0956174905411,9.7572743886747));
#12378=CARTESIAN_POINT('Ctrl Pts',(0.929206149362414,14.080365422028,9.58920247165813));
#12379=CARTESIAN_POINT('Ctrl Pts',(1.11453573938891,14.0696774496551,9.46250263892422));
#12380=CARTESIAN_POINT('Ctrl Pts',(1.40724816783219,14.0505265480937,9.17028693794665));
#12381=CARTESIAN_POINT('Ctrl Pts',(1.53424184696403,14.0408238379775,8.98524545523767));
#12382=CARTESIAN_POINT('Ctrl Pts',(1.70300699643852,14.0296280914589,8.57957694362764));
#12383=CARTESIAN_POINT('Ctrl Pts',(1.744771305208,14.0284021096337,8.35893960919316));
#12384=CARTESIAN_POINT('Ctrl Pts',(1.74519314013823,14.0319894998661,8.15200216623844));
#12385=CARTESIAN_POINT('Ctrl Pts',(1.74561666285586,14.0355912434667,7.94423675389232));
#12386=CARTESIAN_POINT('Ctrl Pts',(1.70443814138898,14.0445195895331,7.72278149953618));
#12387=CARTESIAN_POINT('Ctrl Pts',(1.53638760480237,14.0699025683982,7.31558332529205));
#12388=CARTESIAN_POINT('Ctrl Pts',(1.4095285954262,14.0860885568859,7.12981833652177));
#12389=CARTESIAN_POINT('Ctrl Pts',(1.11673420208023,14.1154783264462,6.83642648344605));
#12390=CARTESIAN_POINT('Ctrl Pts',(0.931224465235098,14.1306073628765,6.70916694867708));
#12391=CARTESIAN_POINT('Ctrl Pts',(0.524335140340142,14.151760030746,6.54026633590998));
#12392=CARTESIAN_POINT('Ctrl Pts',(0.302936623449611,14.1575261279583,6.49863870441721));
#12393=CARTESIAN_POINT('Ctrl Pts',(0.0951965682858559,14.1575261279583,
6.49863870441721));
#12394=CARTESIAN_POINT('Origin',(0.0951965682858563,4.09220368528653E-6,
25.8360815995708));
#12395=CARTESIAN_POINT('',(1.85391052501785,-13.7076189828105,25.8360815995708));
#12396=CARTESIAN_POINT('',(1.85391052501785,-7.5,25.8360815995708));
#12397=CARTESIAN_POINT('',(1.85391052501785,20.,25.8360815995708));
#12398=CARTESIAN_POINT('',(-1.66465324600953,-7.5,25.8360815995708));
#12399=CARTESIAN_POINT('',(0.0951965682858563,-7.5,25.8360815995708));
#12400=CARTESIAN_POINT('',(-1.66465324600953,-13.7074732023021,25.8360815995708));
#12401=CARTESIAN_POINT('',(-1.66465324600953,20.,25.8360815995708));
#12402=CARTESIAN_POINT('Origin',(0.0951965682858563,4.09220368528653E-6,
25.8360815995708));
#12403=CARTESIAN_POINT('Origin',(0.0946286395041643,20.,3.93764471879911));
#12404=CARTESIAN_POINT('',(5.09519656828586,-7.5,25.329954808256));
#12405=CARTESIAN_POINT('',(5.09519656828586,7.5,25.329954808256));
#12406=CARTESIAN_POINT('',(5.09519656828586,20.,25.329954808256));
#12407=CARTESIAN_POINT('Origin',(0.0946286395041643,-7.5,3.93764471879911));
#12408=CARTESIAN_POINT('',(13.9148485158407,-1.53043517371412,21.0150605989476));
#12409=CARTESIAN_POINT('Ctrl Pts',(1.85391052501786,-13.7076189828105,25.8360815995708));
#12410=CARTESIAN_POINT('Ctrl Pts',(2.17648767471965,-13.6666877855093,25.8101663189852));
#12411=CARTESIAN_POINT('Ctrl Pts',(2.49904065381574,-13.6142947682306,25.777060184476));
#12412=CARTESIAN_POINT('Ctrl Pts',(3.72754363797017,-13.3699910032897,25.6234687931974));
#12413=CARTESIAN_POINT('Ctrl Pts',(4.62247333626519,-13.0970219827471,25.4529090529867));
#12414=CARTESIAN_POINT('Ctrl Pts',(7.17708557690186,-12.030828714843,24.8077398984456));
#12415=CARTESIAN_POINT('Ctrl Pts',(8.70490101058748,-10.9780802446545,24.1936108601555));
#12416=CARTESIAN_POINT('Ctrl Pts',(11.1212920908085,-8.58574185129343,22.9873702251227));
#12417=CARTESIAN_POINT('Ctrl Pts',(12.1830463956658,-7.06841765762853,22.303147136569));
#12418=CARTESIAN_POINT('Ctrl Pts',(13.2627850426251,-4.53156635476595,21.5283391995247));
#12419=CARTESIAN_POINT('Ctrl Pts',(13.540303942053,-3.64206254291784,21.3130804475981));
#12420=CARTESIAN_POINT('Ctrl Pts',(13.8061400403014,-2.33638296572343,21.1027786503388));
#12421=CARTESIAN_POINT('Ctrl Pts',(13.8695513851653,-1.93364874310124,21.0517181535856));
#12422=CARTESIAN_POINT('Ctrl Pts',(13.9148485158408,-1.53043517371412,21.0150605989476));
#12423=CARTESIAN_POINT('',(13.9148485158407,1.53044335812149,21.0150605989476));
#12424=CARTESIAN_POINT('',(13.9148485158407,20.,21.0150605989476));
#12425=CARTESIAN_POINT('',(1.85391052501785,13.7076271672179,25.8360815995708));
#12426=CARTESIAN_POINT('Ctrl Pts',(13.9148485158408,1.5304433581215,21.0150605989476));
#12427=CARTESIAN_POINT('Ctrl Pts',(13.8695513851653,1.93365692750862,21.0517181535856));
#12428=CARTESIAN_POINT('Ctrl Pts',(13.8061400403014,2.33639115013081,21.1027786503388));
#12429=CARTESIAN_POINT('Ctrl Pts',(13.5403039420529,3.64207072732521,21.3130804475981));
#12430=CARTESIAN_POINT('Ctrl Pts',(13.2627850426251,4.53157453917333,21.5283391995247));
#12431=CARTESIAN_POINT('Ctrl Pts',(12.1830463956658,7.0684258420359,22.303147136569));
#12432=CARTESIAN_POINT('Ctrl Pts',(11.1212920908085,8.58575003570079,22.9873702251227));
#12433=CARTESIAN_POINT('Ctrl Pts',(8.70490101058748,10.9780884290619,24.1936108601555));
#12434=CARTESIAN_POINT('Ctrl Pts',(7.17708557690186,12.0308368992504,24.8077398984456));
#12435=CARTESIAN_POINT('Ctrl Pts',(4.62247333626519,13.0970301671545,25.4529090529867));
#12436=CARTESIAN_POINT('Ctrl Pts',(3.72754363797016,13.3699991876971,25.6234687931974));
#12437=CARTESIAN_POINT('Ctrl Pts',(2.49904065381574,13.6143029526379,25.777060184476));
#12438=CARTESIAN_POINT('Ctrl Pts',(2.17648767471964,13.6666959699166,25.8101663189852));
#12439=CARTESIAN_POINT('Ctrl Pts',(1.85391052501785,13.7076271672179,25.8360815995708));
#12440=CARTESIAN_POINT('',(1.85391052501785,7.5,25.8360815995708));
#12441=CARTESIAN_POINT('',(1.85391052501785,20.,25.8360815995708));
#12442=CARTESIAN_POINT('Origin',(0.0946286395041643,7.5,3.93764471879911));
#12443=CARTESIAN_POINT('Origin',(0.0946286395041643,20.,3.93764471879911));
#12444=CARTESIAN_POINT('',(-4.90480343171414,-7.5,25.3302202892888));
#12445=CARTESIAN_POINT('Origin',(0.0946286395041643,-7.5,3.93764471879911));
#12446=CARTESIAN_POINT('',(-4.90480343171414,7.5,25.3302202892888));
#12447=CARTESIAN_POINT('',(-4.90480343171414,20.,25.3302202892888));
#12448=CARTESIAN_POINT('',(-1.66465324600953,7.5,25.8360815995708));
#12449=CARTESIAN_POINT('Origin',(0.0946286395041643,7.5,3.93764471879911));
#12450=CARTESIAN_POINT('',(-1.66465324600953,13.7074813867094,25.8360815995708));
#12451=CARTESIAN_POINT('',(-1.66465324600953,20.,25.8360815995708));
#12452=CARTESIAN_POINT('Ctrl Pts',(-1.66465324600953,13.7074813867094,25.8360815995708));
#12453=CARTESIAN_POINT('Ctrl Pts',(-1.98684074890723,13.666572498391,25.8101976225238));
#12454=CARTESIAN_POINT('Ctrl Pts',(-2.30900267606637,13.6142293374932,25.7771403165208));
#12455=CARTESIAN_POINT('Ctrl Pts',(-3.53711118769133,13.3700057780211,25.6236650528541));
#12456=CARTESIAN_POINT('Ctrl Pts',(-4.43203636345268,13.0970405100357,25.4531566824588));
#12457=CARTESIAN_POINT('Ctrl Pts',(-6.98664158061922,12.0308577278043,24.8081401060509));
#12458=CARTESIAN_POINT('Ctrl Pts',(-8.51446121511986,10.9781143124401,24.1941111489798));
#12459=CARTESIAN_POINT('Ctrl Pts',(-10.9308714321239,8.58576963670896,22.9880418512269));
#12460=CARTESIAN_POINT('Ctrl Pts',(-11.9926351420235,7.06843317708346,22.3039048439548));
#12461=CARTESIAN_POINT('Ctrl Pts',(-13.0723782208733,4.53156918261022,21.5291992027477));
#12462=CARTESIAN_POINT('Ctrl Pts',(-13.3498970434732,3.64206232315039,21.3139698195036));
#12463=CARTESIAN_POINT('Ctrl Pts',(-13.7188857908144,1.82973119863964,21.0221044535754));
#12464=CARTESIAN_POINT('Ctrl Pts',(-13.8101407844913,0.90673105293582,20.9462895160591));
#12465=CARTESIAN_POINT('Ctrl Pts',(-13.8101407844913,-0.906722868528451,
20.9462895160591));
#12466=CARTESIAN_POINT('Ctrl Pts',(-13.7188857908144,-1.82972301423227,
21.0221044535754));
#12467=CARTESIAN_POINT('Ctrl Pts',(-13.3498970434732,-3.64205413874302,
21.3139698195036));
#12468=CARTESIAN_POINT('Ctrl Pts',(-13.0723782208733,-4.53156099820285,
21.5291992027477));
#12469=CARTESIAN_POINT('Ctrl Pts',(-11.9926351420235,-7.06842499267609,
22.3039048439548));
#12470=CARTESIAN_POINT('Ctrl Pts',(-10.9308714321239,-8.58576145230159,
22.9880418512269));
#12471=CARTESIAN_POINT('Ctrl Pts',(-8.51446121511986,-10.9781061280328,
24.1941111489798));
#12472=CARTESIAN_POINT('Ctrl Pts',(-6.98664158061922,-12.0308495433969,
24.8081401060509));
#12473=CARTESIAN_POINT('Ctrl Pts',(-4.43203636345268,-13.0970323256283,
25.4531566824588));
#12474=CARTESIAN_POINT('Ctrl Pts',(-3.53711118769134,-13.3699975936137,
25.6236650528541));
#12475=CARTESIAN_POINT('Ctrl Pts',(-2.30900267606638,-13.6142211530858,
25.7771403165208));
#12476=CARTESIAN_POINT('Ctrl Pts',(-1.98684074890723,-13.6665643139837,
25.8101976225238));
#12477=CARTESIAN_POINT('Ctrl Pts',(-1.66465324600953,-13.7074732023021,
25.8360815995708));
#12478=CARTESIAN_POINT('Origin',(0.0951965682858563,4.09220368528653E-6,
-1.66391840042922));
#12479=CARTESIAN_POINT('Origin',(0.0951965682858563,4.09220368528653E-6,
25.8360815995708));
#12480=CARTESIAN_POINT('',(13.9964332854894,1.91230024237248,13.6811463567195));
#12481=CARTESIAN_POINT('Ctrl Pts',(13.9964332854889,1.91230024237026,13.6811463567665));
#12482=CARTESIAN_POINT('Ctrl Pts',(13.9511163435649,1.71995846239176,17.7548302958379));
#12483=CARTESIAN_POINT('Ctrl Pts',(13.9148485158408,1.53044335812149,21.0150605989476));
#12484=CARTESIAN_POINT('',(11.4459127938674,8.25000409220368,13.6811463567195));
#12485=CARTESIAN_POINT('Origin',(0.0951965682858563,4.0922036817656E-6,
13.6811463567195));
#12486=CARTESIAN_POINT('',(11.7275471444307,8.25000409220369,0.574489862137293));
#12487=CARTESIAN_POINT('Ctrl Pts',(11.7275471444307,8.25000409220369,0.574489862137293));
#12488=CARTESIAN_POINT('Ctrl Pts',(11.7222207733811,8.25000409220369,0.823392575266454));
#12489=CARTESIAN_POINT('Ctrl Pts',(11.7168931785629,8.25000409220369,1.07229526221072));
#12490=CARTESIAN_POINT('Ctrl Pts',(11.7115643549194,8.25000409220369,1.32119792284374));
#12491=CARTESIAN_POINT('Ctrl Pts',(11.623358382574,8.25000409220369,5.4411881250697));
#12492=CARTESIAN_POINT('Ctrl Pts',(11.5348159240829,8.25000409220368,9.5611711391444));
#12493=CARTESIAN_POINT('Ctrl Pts',(11.4459127938674,8.25000409220368,13.6811463567195));
#12494=CARTESIAN_POINT('',(11.7275471444307,-8.24999590779632,0.574489862137297));
#12495=CARTESIAN_POINT('Ctrl Pts',(11.7275471444307,-8.24999590779632,0.574489862137297));
#12496=CARTESIAN_POINT('Ctrl Pts',(11.2506528785961,-8.91132535705997,0.941801995911842));
#12497=CARTESIAN_POINT('Ctrl Pts',(10.7233874704347,-9.52161727744828,1.31121249637851));
#12498=CARTESIAN_POINT('Ctrl Pts',(8.94944501462999,-11.2682573787269,2.41723416442409));
#12499=CARTESIAN_POINT('Ctrl Pts',(7.39695628067307,-12.3428102097436,3.18167544610478));
#12500=CARTESIAN_POINT('Ctrl Pts',(4.77843360940769,-13.4402628572067,3.98877045439691));
#12501=CARTESIAN_POINT('Ctrl Pts',(3.85772926770378,-13.723285699755,4.20321806216009));
#12502=CARTESIAN_POINT('Ctrl Pts',(1.98310564117687,-14.0988472144289,4.49284734361978));
#12503=CARTESIAN_POINT('Ctrl Pts',(1.02913009218085,-14.1912194513045,4.56788061831652));
#12504=CARTESIAN_POINT('Ctrl Pts',(-0.837205424454879,-14.1910264736106,
4.57893630299566));
#12505=CARTESIAN_POINT('Ctrl Pts',(-1.79050220705526,-14.0987476035694,
4.51541564045522));
#12506=CARTESIAN_POINT('Ctrl Pts',(-3.66513456872354,-13.7230644103538,
4.24895350849291));
#12507=CARTESIAN_POINT('Ctrl Pts',(-4.58652368156226,-13.4398199148439,
4.04616337164375));
#12508=CARTESIAN_POINT('Ctrl Pts',(-7.20822347504013,-12.340360202428,3.27354943135428));
#12509=CARTESIAN_POINT('Ctrl Pts',(-8.7643920193079,-11.2624168750667,2.53153132261272));
#12510=CARTESIAN_POINT('Ctrl Pts',(-11.2319892354444,-8.8269552131712,1.03862052793401));
#12511=CARTESIAN_POINT('Ctrl Pts',(-12.317306699732,-7.28274628710442,0.167204139697448));
#12512=CARTESIAN_POINT('Ctrl Pts',(-13.4306122032903,-4.6928986142151,-0.858100732123217));
#12513=CARTESIAN_POINT('Ctrl Pts',(-13.7190471318454,-3.78298207865309,
-1.15053717027747));
#12514=CARTESIAN_POINT('Ctrl Pts',(-14.1062637700055,-1.91424092738689,
-1.55431913138643));
#12515=CARTESIAN_POINT('Ctrl Pts',(-14.2048034317141,-0.954989281852873,
-1.66391840042921));
#12516=CARTESIAN_POINT('Ctrl Pts',(-14.2048034317141,0.954997466260247,
-1.66391840042921));
#12517=CARTESIAN_POINT('Ctrl Pts',(-14.1062637700055,1.91424911179426,-1.55431913138642));
#12518=CARTESIAN_POINT('Ctrl Pts',(-13.7190471318454,3.78299026306046,-1.15053717027747));
#12519=CARTESIAN_POINT('Ctrl Pts',(-13.4306122032903,4.69290679862247,-0.85810073212322));
#12520=CARTESIAN_POINT('Ctrl Pts',(-12.317306699732,7.28275447151178,0.167204139697442));
#12521=CARTESIAN_POINT('Ctrl Pts',(-11.2319892354444,8.82696339757856,1.03862052793401));
#12522=CARTESIAN_POINT('Ctrl Pts',(-8.7643920193079,11.2624250594741,2.53153132261272));
#12523=CARTESIAN_POINT('Ctrl Pts',(-7.20822347504013,12.3403683868354,3.27354943135428));
#12524=CARTESIAN_POINT('Ctrl Pts',(-4.58652368156226,13.4398280992513,4.04616337164375));
#12525=CARTESIAN_POINT('Ctrl Pts',(-3.66513456872355,13.7230725947612,4.24895350849291));
#12526=CARTESIAN_POINT('Ctrl Pts',(-1.79050220705526,14.0987557879767,4.51541564045522));
#12527=CARTESIAN_POINT('Ctrl Pts',(-0.837205424454882,14.191034658018,4.57893630299566));
#12528=CARTESIAN_POINT('Ctrl Pts',(1.03171319044408,14.1912279028023,4.56786531671633));
#12529=CARTESIAN_POINT('Ctrl Pts',(1.98817223795939,14.0983467992742,4.49243379841232));
#12530=CARTESIAN_POINT('Ctrl Pts',(3.86732265571208,13.720861540725,4.2013637484486));
#12531=CARTESIAN_POINT('Ctrl Pts',(4.79007085667628,13.4364250401153,3.98587473350674));
#12532=CARTESIAN_POINT('Ctrl Pts',(7.41380568479443,12.3336701876795,3.1750837142893));
#12533=CARTESIAN_POINT('Ctrl Pts',(8.96853555697387,11.2541395041803,2.40738046212495));
#12534=CARTESIAN_POINT('Ctrl Pts',(10.7357556493519,9.50728123601757,1.3025507908185));
#12535=CARTESIAN_POINT('Ctrl Pts',(11.256192956559,8.90365088103174,0.937534932951304));
#12536=CARTESIAN_POINT('Ctrl Pts',(11.7275471444307,8.25000409220369,0.574489862137297));
#12537=CARTESIAN_POINT('',(11.4459127938674,-8.24999590779632,13.6811463567195));
#12538=CARTESIAN_POINT('Ctrl Pts',(11.4459127938674,-8.24999590779632,13.6811463567195));
#12539=CARTESIAN_POINT('Ctrl Pts',(11.5348159240829,-8.24999590779632,9.56117113914441));
#12540=CARTESIAN_POINT('Ctrl Pts',(11.623358382574,-8.24999590779632,5.44118812506971));
#12541=CARTESIAN_POINT('Ctrl Pts',(11.7115643549194,-8.24999590779632,1.32119792284375));
#12542=CARTESIAN_POINT('Ctrl Pts',(11.7168931785629,-8.24999590779632,1.07229526221074));
#12543=CARTESIAN_POINT('Ctrl Pts',(11.7222207733811,-8.24999590779632,0.823392575266463));
#12544=CARTESIAN_POINT('Ctrl Pts',(11.7275471444307,-8.24999590779632,0.574489862137297));
#12545=CARTESIAN_POINT('',(13.9964332854894,-1.9122920579651,13.6811463567195));
#12546=CARTESIAN_POINT('Origin',(0.0951965682858563,4.0922036817656E-6,
13.6811463567195));
#12547=CARTESIAN_POINT('Ctrl Pts',(13.9148485158427,-1.53043517372403,21.015060598777));
#12548=CARTESIAN_POINT('Ctrl Pts',(13.9511163435661,-1.71995027798942,17.7548302957312));
#12549=CARTESIAN_POINT('Ctrl Pts',(13.9964332854889,-1.91229205796288,13.6811463567667));
#12550=CARTESIAN_POINT('Origin',(14.1653954217721,39.6000040922037,-1.5073970811911));
#12551=CARTESIAN_POINT('',(13.9964332854894,39.6000040922037,13.6811463567195));
#12552=CARTESIAN_POINT('Origin',(0.0951965682858563,4.09220368528653E-6,
25.8360815995708));
#12553=CARTESIAN_POINT('',(0.0951965682858563,7.5,25.8360815995708));
#12554=CARTESIAN_POINT('Origin',(-0.0188334087686722,39.6000040922037,-14.6762492641943));
#12555=CARTESIAN_POINT('',(-8.70480343171414,-8.24999590779632,2.50270369460076));
#12556=CARTESIAN_POINT('',(-8.70480343171414,8.25000409220368,2.50270369460076));
#12557=CARTESIAN_POINT('',(-8.70480343171414,39.6000040922037,2.50270369460077));
#12558=CARTESIAN_POINT('Origin',(-0.0188334087686722,-8.24999590779631,
-14.6762492641943));
#12559=CARTESIAN_POINT('Origin',(-0.0188334087686722,8.25000409220369,-14.6762492641943));
#12560=CARTESIAN_POINT('Origin',(17.6951965682859,-8.24999590779631,-17.008983157578));
#12561=CARTESIAN_POINT('',(-8.70480343171414,-8.24999590779632,13.6811463567195));
#12562=CARTESIAN_POINT('',(-8.70480343171414,-8.24999590779631,-17.008983157578));
#12563=CARTESIAN_POINT('',(17.6951965682859,-8.24999590779632,13.6811463567195));
#12564=CARTESIAN_POINT('Origin',(17.6951965682859,8.25000409220369,-17.0089831575779));
#12565=CARTESIAN_POINT('',(-8.70480343171414,8.25000409220368,13.6811463567195));
#12566=CARTESIAN_POINT('',(17.6951965682859,8.25000409220368,13.6811463567195));
#12567=CARTESIAN_POINT('',(-8.70480343171414,8.25000409220369,-17.0089831575779));
#12568=CARTESIAN_POINT('Origin',(17.6951965682859,8.25000409220368,13.6811463567195));
#12569=CARTESIAN_POINT('',(-8.70480343171414,8.25000409220368,13.6811463567195));
#12570=CARTESIAN_POINT('Origin',(-8.70480343171414,4.09220368528653E-6,
-1.66391840042922));
#12571=CARTESIAN_POINT('Origin',(5.09519656828586,-7.5,14.732185266773));
#12572=CARTESIAN_POINT('',(5.09519656828586,-7.5,36.732185266773));
#12573=CARTESIAN_POINT('',(5.09519656828586,-7.5,14.732185266773));
#12574=CARTESIAN_POINT('',(5.09519656828586,7.5,36.732185266773));
#12575=CARTESIAN_POINT('',(5.09519656828586,7.5,14.732185266773));
#12576=CARTESIAN_POINT('',(5.09519656828586,-7.5,36.732185266773));
#12577=CARTESIAN_POINT('Origin',(-4.90480343171414,-7.5,36.732185266773));
#12578=CARTESIAN_POINT('',(-4.90480343171414,7.5,36.732185266773));
#12579=CARTESIAN_POINT('',(-4.90480343171414,7.5,36.732185266773));
#12580=CARTESIAN_POINT('',(-4.90480343171414,-7.5,36.732185266773));
#12581=CARTESIAN_POINT('',(-4.90480343171414,-7.5,36.732185266773));
#12582=CARTESIAN_POINT('',(-4.90480343171414,-7.5,36.732185266773));
#12583=CARTESIAN_POINT('Origin',(-4.90480343171414,-7.5,14.732185266773));
#12584=CARTESIAN_POINT('',(-4.90480343171414,7.5,14.732185266773));
#12585=CARTESIAN_POINT('',(-4.90480343171414,-7.5,14.732185266773));
#12586=CARTESIAN_POINT('Origin',(0.,-7.5,0.));
#12587=CARTESIAN_POINT('Origin',(0.,7.5,0.));
#12588=CARTESIAN_POINT('',(0.,0.,0.));
#12589=CARTESIAN_POINT('Origin',(0.110247934021453,18.,10.8869317850633));
#12590=CARTESIAN_POINT('',(0.110247934021453,-8.24965010070131,12.3869317850633));
#12591=CARTESIAN_POINT('Origin',(0.110247934021453,-8.24965010070131,10.8869317850633));
#12592=CARTESIAN_POINT('',(0.110247933887646,-14.0552557433871,12.3869317850633));
#12593=CARTESIAN_POINT('',(0.110247934021453,18.,12.3869317850633));
#12594=CARTESIAN_POINT('',(0.110247934021453,-14.1076210252064,9.3869317850633));
#12595=CARTESIAN_POINT('Ctrl Pts',(0.110247933753838,-14.0552557433871,
12.3869317850633));
#12596=CARTESIAN_POINT('Ctrl Pts',(-0.0779989827009714,-14.0549118893516,
12.3869317850297));
#12597=CARTESIAN_POINT('Ctrl Pts',(-0.278728344791251,-14.0510324275907,
12.3493319245718));
#12598=CARTESIAN_POINT('Ctrl Pts',(-0.647959467681628,-14.0379478709213,
12.1965290487721));
#12599=CARTESIAN_POINT('Ctrl Pts',(-0.816468494212286,-14.0289559136302,
12.0813250316921));
#12600=CARTESIAN_POINT('Ctrl Pts',(-1.08260740435852,-14.0130041171202,
11.8156060213132));
#12601=CARTESIAN_POINT('Ctrl Pts',(-1.19805838607211,-14.0050121842533,
11.6473460303996));
#12602=CARTESIAN_POINT('Ctrl Pts',(-1.3514541799802,-13.9960274725997,11.2784955234755));
#12603=CARTESIAN_POINT('Ctrl Pts',(-1.38939360404563,-13.9952553156971,
11.0778974256665));
#12604=CARTESIAN_POINT('Ctrl Pts',(-1.39010647607766,-14.0017963063311,
10.7009453898944));
#12605=CARTESIAN_POINT('Ctrl Pts',(-1.35266265154803,-14.0095718793367,
10.4996613198593));
#12606=CARTESIAN_POINT('Ctrl Pts',(-1.19987566293113,-14.0314540986523,
10.1295270026253));
#12607=CARTESIAN_POINT('Ctrl Pts',(-1.08454283481342,-14.0453388880625,
9.96065940627607));
#12608=CARTESIAN_POINT('Ctrl Pts',(-0.818352054767195,-14.0705968835703,
9.69395625658189));
#12609=CARTESIAN_POINT('Ctrl Pts',(-0.649705142487691,-14.0836248485775,
9.5782824456212));
#12610=CARTESIAN_POINT('Ctrl Pts',(-0.279839795725651,-14.1020716632627,
9.42476786050772));
#12611=CARTESIAN_POINT('Ctrl Pts',(-0.078606279092388,-14.1072765984644,
9.38693779445533));
#12612=CARTESIAN_POINT('Ctrl Pts',(0.110216109641043,-14.1076209672601,
9.3869317853165));
#12613=CARTESIAN_POINT('Ctrl Pts',(0.110232021787044,-14.1076209962489,
9.3869317850633));
#12614=CARTESIAN_POINT('Ctrl Pts',(0.110247934021453,-14.1076210252064,
9.3869317850633));
#12615=CARTESIAN_POINT('Ctrl Pts',(0.110247934021453,-14.1076210252064,
9.3869317850633));
#12616=CARTESIAN_POINT('Ctrl Pts',(0.299018164756681,-14.1079645552822,
9.3869317850633));
#12617=CARTESIAN_POINT('Ctrl Pts',(0.500231125056626,-14.1034945808851,
9.42474185766269));
#12618=CARTESIAN_POINT('Ctrl Pts',(0.870098969070737,-14.0864013169578,
9.57822271524134));
#12619=CARTESIAN_POINT('Ctrl Pts',(1.03876516505625,-14.0739913371949,9.69389031798828));
#12620=CARTESIAN_POINT('Ctrl Pts',(1.30499104641839,-14.0497109843586,9.96059468363198));
#12621=CARTESIAN_POINT('Ctrl Pts',(1.42033561388508,-14.0362517791226,10.1294648498598));
#12622=CARTESIAN_POINT('Ctrl Pts',(1.57314021718156,-14.0149355408367,10.4995921319432));
#12623=CARTESIAN_POINT('Ctrl Pts',(1.61059047387225,-14.0072999254605,10.700866003491));
#12624=CARTESIAN_POINT('Ctrl Pts',(1.61024542921315,-14.0040223989729,10.8896730290548));
#12625=CARTESIAN_POINT('Ctrl Pts',(1.60990162279029,-14.000756634302,11.0778024968157));
#12626=CARTESIAN_POINT('Ctrl Pts',(1.57197504847848,-14.0013878345693,11.2784068501416));
#12627=CARTESIAN_POINT('Ctrl Pts',(1.41859248113633,-14.0098055316953,11.6472826572499));
#12628=CARTESIAN_POINT('Ctrl Pts',(1.30314144421112,-14.0173717863179,11.8155611648083));
#12629=CARTESIAN_POINT('Ctrl Pts',(1.03699817477234,-14.032345318826,12.0812980188678));
#12630=CARTESIAN_POINT('Ctrl Pts',(0.868493391579155,-14.0407189153297,
12.196505971612));
#12631=CARTESIAN_POINT('Ctrl Pts',(0.499264482529693,-14.052452711895,12.3493225855658));
#12632=CARTESIAN_POINT('Ctrl Pts',(0.298531336987817,-14.0555991292645,
12.3869257938369));
#12633=CARTESIAN_POINT('Ctrl Pts',(0.110279758313445,-14.0552558014956,
12.3869317848101));
#12634=CARTESIAN_POINT('Ctrl Pts',(0.110263846078239,-14.0552557724528,
12.3869317850633));
#12635=CARTESIAN_POINT('Ctrl Pts',(0.110247933753838,-14.0552557433871,
12.3869317850633));
#12636=CARTESIAN_POINT('Origin',(0.110247934021453,18.,10.8869317850633));
#12637=CARTESIAN_POINT('',(0.110247934021807,14.1083208238043,9.38693178505972));
#12638=CARTESIAN_POINT('',(0.110247933887645,14.0559555419845,12.3869317850633));
#12639=CARTESIAN_POINT('Ctrl Pts',(0.110247934021808,14.1083208238038,9.3869317850633));
#12640=CARTESIAN_POINT('Ctrl Pts',(0.110232021787281,14.1083207948462,9.3869317850633));
#12641=CARTESIAN_POINT('Ctrl Pts',(0.11021610964116,14.1083207658575,9.3869317853165));
#12642=CARTESIAN_POINT('Ctrl Pts',(-0.0786062790923889,14.1079763970618,
9.38693779445533));
#12643=CARTESIAN_POINT('Ctrl Pts',(-0.279839795725652,14.1027714618601,
9.42476786050772));
#12644=CARTESIAN_POINT('Ctrl Pts',(-0.649705142487692,14.0843246471749,
9.57828244562119));
#12645=CARTESIAN_POINT('Ctrl Pts',(-0.818352054767195,14.0712966821677,
9.69395625658189));
#12646=CARTESIAN_POINT('Ctrl Pts',(-1.08454283481342,14.0460386866599,9.96065940627607));
#12647=CARTESIAN_POINT('Ctrl Pts',(-1.19987566293113,14.0321538972497,10.1295270026253));
#12648=CARTESIAN_POINT('Ctrl Pts',(-1.35266265154803,14.0102716779341,10.4996613198593));
#12649=CARTESIAN_POINT('Ctrl Pts',(-1.39010647607766,14.0024961049285,10.7009453898944));
#12650=CARTESIAN_POINT('Ctrl Pts',(-1.38939360404563,13.9959551142944,11.0778974256665));
#12651=CARTESIAN_POINT('Ctrl Pts',(-1.3514541799802,13.9967272711971,11.2784955234755));
#12652=CARTESIAN_POINT('Ctrl Pts',(-1.19805838607211,14.0057119828507,11.6473460303996));
#12653=CARTESIAN_POINT('Ctrl Pts',(-1.08260740435852,14.0137039157176,11.8156060213132));
#12654=CARTESIAN_POINT('Ctrl Pts',(-0.816468494212286,14.0296557122276,
12.0813250316921));
#12655=CARTESIAN_POINT('Ctrl Pts',(-0.647959467681628,14.0386476695187,
12.1965290487721));
#12656=CARTESIAN_POINT('Ctrl Pts',(-0.278728344791252,14.051732226188,12.3493319245718));
#12657=CARTESIAN_POINT('Ctrl Pts',(-0.0779989827009722,14.055611687949,
12.3869317850297));
#12658=CARTESIAN_POINT('Ctrl Pts',(0.110247933753837,14.0559555419845,12.3869317850633));
#12659=CARTESIAN_POINT('',(0.110247934021453,8.25034989929869,12.3869317850633));
#12660=CARTESIAN_POINT('',(0.110247934021453,18.,12.3869317850633));
#12661=CARTESIAN_POINT('Origin',(0.110247934021453,8.25034989929869,10.8869317850633));
#12662=CARTESIAN_POINT('Ctrl Pts',(0.110247933753837,14.0559555419845,12.3869317850633));
#12663=CARTESIAN_POINT('Ctrl Pts',(0.110263846078238,14.0559555710501,12.3869317850633));
#12664=CARTESIAN_POINT('Ctrl Pts',(0.110279758313445,14.055955600093,12.3869317848101));
#12665=CARTESIAN_POINT('Ctrl Pts',(0.298531336987817,14.0562989278619,12.3869257938369));
#12666=CARTESIAN_POINT('Ctrl Pts',(0.499264482529694,14.0531525104924,12.3493225855658));
#12667=CARTESIAN_POINT('Ctrl Pts',(0.868493391579156,14.0414187139271,12.196505971612));
#12668=CARTESIAN_POINT('Ctrl Pts',(1.03699817477234,14.0330451174234,12.0812980188678));
#12669=CARTESIAN_POINT('Ctrl Pts',(1.30314144421112,14.0180715849152,11.8155611648083));
#12670=CARTESIAN_POINT('Ctrl Pts',(1.41859248113633,14.0105053302927,11.6472826572499));
#12671=CARTESIAN_POINT('Ctrl Pts',(1.57197504847848,14.0020876331667,11.2784068501416));
#12672=CARTESIAN_POINT('Ctrl Pts',(1.60990162279029,14.0014564328994,11.0778024968157));
#12673=CARTESIAN_POINT('Ctrl Pts',(1.61024542921315,14.0047221975703,10.8896730290548));
#12674=CARTESIAN_POINT('Ctrl Pts',(1.61059047387225,14.0079997240579,10.700866003491));
#12675=CARTESIAN_POINT('Ctrl Pts',(1.57314021718156,14.0156353394341,10.4995921319432));
#12676=CARTESIAN_POINT('Ctrl Pts',(1.42033561388508,14.03695157772,10.1294648498598));
#12677=CARTESIAN_POINT('Ctrl Pts',(1.30499104641839,14.050410782956,9.96059468363198));
#12678=CARTESIAN_POINT('Ctrl Pts',(1.03876516505625,14.0746911357923,9.69389031798828));
#12679=CARTESIAN_POINT('Ctrl Pts',(0.870098969070735,14.0871011155552,9.57822271524134));
#12680=CARTESIAN_POINT('Ctrl Pts',(0.500231125056741,14.1041943794824,9.42474185766273));
#12681=CARTESIAN_POINT('Ctrl Pts',(0.299018164756932,14.1086643538796,9.38693178506334));
#12682=CARTESIAN_POINT('Ctrl Pts',(0.110247934021808,14.1083208238038,9.3869317850633));
#12683=CARTESIAN_POINT('Origin',(-17.8485597402224,-0.120323143610449,-16.1677081946201));
#12684=CARTESIAN_POINT('',(-16.497528189245,2.37951225022575,-1.54552565392526));
#12685=CARTESIAN_POINT('',(-16.497528189245,-2.62015853744665,-1.54552565392526));
#12686=CARTESIAN_POINT('Ctrl Pts',(-16.4975281892429,2.37951225022459,-1.54552565392739));
#12687=CARTESIAN_POINT('Ctrl Pts',(-16.420741563328,2.33801305609358,-1.62231227984189));
#12688=CARTESIAN_POINT('Ctrl Pts',(-16.3240357866784,2.27985744112584,-1.69185037854978));
#12689=CARTESIAN_POINT('Ctrl Pts',(-16.0647935003745,2.10171647680498,-1.83077158616984));
#12690=CARTESIAN_POINT('Ctrl Pts',(-15.8578857100574,1.92056821996525,-1.86953234897271));
#12691=CARTESIAN_POINT('Ctrl Pts',(-15.4883556328401,1.49633440199585,-1.86488639419025));
#12692=CARTESIAN_POINT('Ctrl Pts',(-15.3080382336862,1.19791710112843,-1.79698849462938));
#12693=CARTESIAN_POINT('Ctrl Pts',(-15.0674088041674,0.555842639994981,
-1.66403388485253));
#12694=CARTESIAN_POINT('Ctrl Pts',(-15.0069997376864,0.210870575808918,
-1.60558828241371));
#12695=CARTESIAN_POINT('Ctrl Pts',(-15.0069997376864,-0.451516863029818,
-1.60558828241371));
#12696=CARTESIAN_POINT('Ctrl Pts',(-15.0674088041674,-0.79648892721588,
-1.66403388485253));
#12697=CARTESIAN_POINT('Ctrl Pts',(-15.3080382336862,-1.43856338834933,
-1.79698849462938));
#12698=CARTESIAN_POINT('Ctrl Pts',(-15.4883556328401,-1.73698068921675,
-1.86488639419025));
#12699=CARTESIAN_POINT('Ctrl Pts',(-15.8578857100574,-2.16121450718615,
-1.86953234897271));
#12700=CARTESIAN_POINT('Ctrl Pts',(-16.0647935003745,-2.34236276402588,
-1.83077158616984));
#12701=CARTESIAN_POINT('Ctrl Pts',(-16.3240357866792,-2.52050372834728,
-1.69185037854936));
#12702=CARTESIAN_POINT('Ctrl Pts',(-16.4207415633297,-2.57865934331552,
-1.62231227984055));
#12703=CARTESIAN_POINT('Ctrl Pts',(-16.497528189245,-2.62015853744664,-1.54552565392525));
#12704=CARTESIAN_POINT('',(-17.1330436691154,-2.87032314361045,-0.910010174054937));
#12705=CARTESIAN_POINT('Origin',(-17.8485597402078,-0.120323143639212,-0.194494102961751));
#12706=CARTESIAN_POINT('',(-17.1330436691154,-2.87032314361045,-3.73667605240598));
#12707=CARTESIAN_POINT('',(-17.1330436691154,-2.87032314361045,-16.1677081946201));
#12708=CARTESIAN_POINT('',(-18.5640758113294,-2.87032314361045,-5.16770819462005));
#12709=CARTESIAN_POINT('Origin',(-17.8485597402224,-0.120323143607889,-4.45219212351302));
#12710=CARTESIAN_POINT('',(-18.5640758113294,-2.87032314361045,1.43229180537995));
#12711=CARTESIAN_POINT('',(-18.5640758113294,-2.87032314361045,-16.1677081946201));
#12712=CARTESIAN_POINT('',(-18.5640758113294,2.62967685638955,1.43229180537995));
#12713=CARTESIAN_POINT('Origin',(-17.8485597402224,-0.120323143610436,2.14780787648699));
#12714=CARTESIAN_POINT('',(-18.5640758113294,2.62967685638955,-5.16770819462005));
#12715=CARTESIAN_POINT('',(-18.5640758113294,2.62967685638955,-16.1677081946201));
#12716=CARTESIAN_POINT('',(-17.1330436691154,2.62967685638955,-3.73667605240598));
#12717=CARTESIAN_POINT('Origin',(-17.8485597402223,-0.120323143614262,-4.45219212351302));
#12718=CARTESIAN_POINT('',(-17.1330436691154,2.62967685638955,-0.910010174054937));
#12719=CARTESIAN_POINT('',(-17.1330436691154,2.62967685638955,-16.1677081946201));
#12720=CARTESIAN_POINT('Origin',(-17.8485597402879,-0.120323143780666,-0.194494102881747));
#12721=CARTESIAN_POINT('Origin',(-19.7031631078554,-6.08245867427902,-3.00679549114607));
#12722=CARTESIAN_POINT('',(-19.7031631078554,5.84154132572098,-4.10679549114607));
#12723=CARTESIAN_POINT('Origin',(-19.7031631078554,5.84154132572098,-3.00679549114607));
#12724=CARTESIAN_POINT('',(-19.7031631078554,4.74181238705812,-4.10679549114607));
#12725=CARTESIAN_POINT('',(-19.7031631078554,-6.08245867427902,-4.10679549114607));
#12726=CARTESIAN_POINT('Origin',(-19.7031631078554,4.74181238705812,-3.00679549114607));
#12727=CARTESIAN_POINT('Origin',(-19.7031631078554,-6.08245867427902,-3.00679549114607));
#12728=CARTESIAN_POINT('',(-19.7031631078554,-4.98245867427902,-4.10679549114607));
#12729=CARTESIAN_POINT('Origin',(-19.7031631078554,-4.98245867427902,-3.00679549114607));
#12730=CARTESIAN_POINT('',(-19.7031631078554,-6.08245867427902,-4.10679549114607));
#12731=CARTESIAN_POINT('',(-19.7031631078554,-6.08245867427902,-4.10679549114607));
#12732=CARTESIAN_POINT('Origin',(-19.7031631078554,-6.08245867427902,-3.00679549114607));
#12733=CARTESIAN_POINT('Origin',(-19.7031631078554,-6.08245867427902,-3.00679549114607));
#12734=CARTESIAN_POINT('',(-19.7031631078554,2.62967685638955,-4.10679549114607));
#12735=CARTESIAN_POINT('Origin',(-19.7031631078554,2.62967685638955,-3.00679549114607));
#12736=CARTESIAN_POINT('',(-19.7031631078554,-2.87032314361045,-4.10679549114607));
#12737=CARTESIAN_POINT('',(-19.7031631078554,-6.08245867427902,-4.10679549114607));
#12738=CARTESIAN_POINT('Origin',(-19.7031631078554,-2.87032314361045,-3.00679549114607));
#12739=CARTESIAN_POINT('Origin',(0.135922068665986,0.000349899298694283,
-1.61306821493671));
#12740=CARTESIAN_POINT('',(-5.08045717850762,-13.2101970980443,3.93608070944324));
#12741=CARTESIAN_POINT('',(-13.2505381529841,-4.98245867427902,-0.68247630754827));
#12742=CARTESIAN_POINT('Ctrl Pts',(-5.08045717850762,-13.2101970980444,
3.93608070944324));
#12743=CARTESIAN_POINT('Ctrl Pts',(-5.19427083564475,-13.1658432312101,
3.90479457078127));
#12744=CARTESIAN_POINT('Ctrl Pts',(-5.30737084438806,-13.1200941149079,
3.87257838053821));
#12745=CARTESIAN_POINT('Ctrl Pts',(-7.16749797466,-12.340014395333,3.32439961684679));
#12746=CARTESIAN_POINT('Ctrl Pts',(-8.72366651892778,-11.2620710679717,
2.58238150810523));
#12747=CARTESIAN_POINT('Ctrl Pts',(-11.1912637350643,-8.82660940607619,
1.08947071342651));
#12748=CARTESIAN_POINT('Ctrl Pts',(-12.2765811993519,-7.2824004800094,0.21805432518995));
#12749=CARTESIAN_POINT('Ctrl Pts',(-13.1000234307682,-5.36685264522708,
-0.540299360151207));
#12750=CARTESIAN_POINT('Ctrl Pts',(-13.1773264791433,-5.17565684815307,
-0.612785264279329));
#12751=CARTESIAN_POINT('Ctrl Pts',(-13.2505381529841,-4.98245867427907,
-0.682476307548427));
#12752=CARTESIAN_POINT('',(-0.117610192876321,-14.14538010659,7.09490065582709));
#12753=CARTESIAN_POINT('Ctrl Pts',(-5.08045717850762,-13.2101970980444,
3.93608070944324));
#12754=CARTESIAN_POINT('Ctrl Pts',(-4.64036715107621,-13.3817028291032,
4.05705667988745));
#12755=CARTESIAN_POINT('Ctrl Pts',(-4.20677536912925,-13.5243909716407,
4.20923394033941));
#12756=CARTESIAN_POINT('Ctrl Pts',(-3.28371616224739,-13.7831397146222,
4.60459023494974));
#12757=CARTESIAN_POINT('Ctrl Pts',(-2.73813134372595,-13.9017566032157,
4.8919833150883));
#12758=CARTESIAN_POINT('Ctrl Pts',(-1.70519120635403,-14.0638413625729,
5.57389167932221));
#12759=CARTESIAN_POINT('Ctrl Pts',(-1.21811780812576,-14.1085223634017,
5.96854508266688));
#12760=CARTESIAN_POINT('Ctrl Pts',(-0.56724899223391,-14.1409328592556,
6.59350219068028));
#12761=CARTESIAN_POINT('Ctrl Pts',(-0.33704980837108,-14.1459457009925,
6.83721828261811));
#12762=CARTESIAN_POINT('Ctrl Pts',(-0.117610192876322,-14.14538010659,7.09490065582709));
#12763=CARTESIAN_POINT('',(13.9997902889911,-1.74673802437828,17.0911694938297));
#12764=CARTESIAN_POINT('Ctrl Pts',(-0.117610192876319,-14.14538010659,7.09490065582709));
#12765=CARTESIAN_POINT('Ctrl Pts',(0.287626138302845,-14.1443356306413,
7.57075939853091));
#12766=CARTESIAN_POINT('Ctrl Pts',(0.703875256497269,-14.1263201117739,
8.03375426636872));
#12767=CARTESIAN_POINT('Ctrl Pts',(2.81839943242586,-13.9381054957977,10.2645152922982));
#12768=CARTESIAN_POINT('Ctrl Pts',(4.66337005253943,-13.4890535959015,11.8309862161255));
#12769=CARTESIAN_POINT('Ctrl Pts',(7.56897014261126,-11.9529562948628,13.8505592189385));
#12770=CARTESIAN_POINT('Ctrl Pts',(8.64240851599456,-11.2215374031172,14.5111965660852));
#12771=CARTESIAN_POINT('Ctrl Pts',(10.5894885169921,-9.40644175625714,15.5873518377379));
#12772=CARTESIAN_POINT('Ctrl Pts',(11.4595922188052,-8.32118933554518,16.0066065835401));
#12773=CARTESIAN_POINT('Ctrl Pts',(12.7253532066206,-6.19615494318079,16.5792764506805));
#12774=CARTESIAN_POINT('Ctrl Pts',(13.2509932310767,-5.00707161202048,16.7956436259973));
#12775=CARTESIAN_POINT('Ctrl Pts',(13.7806562363602,-3.09709539960396,17.0067163827827));
#12776=CARTESIAN_POINT('Ctrl Pts',(13.9157062376927,-2.41849085402253,17.058858010685));
#12777=CARTESIAN_POINT('Ctrl Pts',(13.9997902889911,-1.74673802437828,17.0911694938297));
#12778=CARTESIAN_POINT('',(13.9019434616744,-1.21975671714985,25.8869317850633));
#12779=CARTESIAN_POINT('Ctrl Pts',(13.9019434616756,-1.21975671715783,25.8869317849523));
#12780=CARTESIAN_POINT('Ctrl Pts',(13.9421779524689,-1.48088863696913,22.2701255314285));
#12781=CARTESIAN_POINT('Ctrl Pts',(13.9997902889911,-1.74673802437823,17.0911694938297));
#12782=CARTESIAN_POINT('',(13.9019434616744,1.22045651574723,25.8869317850633));
#12783=CARTESIAN_POINT('Origin',(0.135922068665986,0.000349899298694283,
25.8869317850633));
#12784=CARTESIAN_POINT('',(13.9997902889911,1.74743782297565,17.0911694938297));
#12785=CARTESIAN_POINT('Ctrl Pts',(13.9997902889911,1.74743782297562,17.0911694938297));
#12786=CARTESIAN_POINT('Ctrl Pts',(13.942177952468,1.48158843556245,22.2701255315078));
#12787=CARTESIAN_POINT('Ctrl Pts',(13.9019434616744,1.2204565157472,25.8869317850633));
#12788=CARTESIAN_POINT('',(-0.117610192876318,14.1460799051874,7.09490065582708));
#12789=CARTESIAN_POINT('Ctrl Pts',(13.9997902889911,1.74743782297566,17.0911694938297));
#12790=CARTESIAN_POINT('Ctrl Pts',(13.9157062376927,2.41919065261991,17.058858010685));
#12791=CARTESIAN_POINT('Ctrl Pts',(13.7806562363602,3.09779519820135,17.0067163827827));
#12792=CARTESIAN_POINT('Ctrl Pts',(13.2509932310767,5.00777141061787,16.7956436259973));
#12793=CARTESIAN_POINT('Ctrl Pts',(12.7253532066206,6.19685474177818,16.5792764506805));
#12794=CARTESIAN_POINT('Ctrl Pts',(11.4595922188052,8.32188913414257,16.0066065835401));
#12795=CARTESIAN_POINT('Ctrl Pts',(10.5894885169921,9.40714155485452,15.5873518377379));
#12796=CARTESIAN_POINT('Ctrl Pts',(8.64240851599456,11.2222372017146,14.5111965660852));
#12797=CARTESIAN_POINT('Ctrl Pts',(7.56897014261126,11.9536560934602,13.8505592189385));
#12798=CARTESIAN_POINT('Ctrl Pts',(4.66337005253943,13.4897533944989,11.8309862161255));
#12799=CARTESIAN_POINT('Ctrl Pts',(2.81839943242586,13.9388052943951,10.2645152922982));
#12800=CARTESIAN_POINT('Ctrl Pts',(0.703875256497267,14.1270199103713,8.03375426636873));
#12801=CARTESIAN_POINT('Ctrl Pts',(0.287626138302846,14.1450354292387,7.57075939853092));
#12802=CARTESIAN_POINT('Ctrl Pts',(-0.117610192876319,14.1460799051874,
7.09490065582709));
#12803=CARTESIAN_POINT('',(-5.08045717850761,13.2108968966417,3.93608070944324));
#12804=CARTESIAN_POINT('Ctrl Pts',(-0.117610192876326,14.1460799051874,
7.09490065582709));
#12805=CARTESIAN_POINT('Ctrl Pts',(-0.337049808371082,14.1466454995899,
6.83721828261811));
#12806=CARTESIAN_POINT('Ctrl Pts',(-0.56724899223391,14.141632657853,6.59350219068028));
#12807=CARTESIAN_POINT('Ctrl Pts',(-1.21811780812576,14.1092221619991,5.96854508266688));
#12808=CARTESIAN_POINT('Ctrl Pts',(-1.70519120635403,14.0645411611703,5.57389167932221));
#12809=CARTESIAN_POINT('Ctrl Pts',(-2.73813134372595,13.9024564018131,4.8919833150883));
#12810=CARTESIAN_POINT('Ctrl Pts',(-3.28371616224739,13.7838395132195,4.60459023494974));
#12811=CARTESIAN_POINT('Ctrl Pts',(-4.20677536912925,13.5250907702381,4.20923394033941));
#12812=CARTESIAN_POINT('Ctrl Pts',(-4.6403671510762,13.3824026277006,4.05705667988745));
#12813=CARTESIAN_POINT('Ctrl Pts',(-5.0804571785076,13.2108968966417,3.93608070944325));
#12814=CARTESIAN_POINT('',(-13.3394911057634,4.74181001551124,-0.767702265509899));
#12815=CARTESIAN_POINT('Ctrl Pts',(-13.3394914716453,4.74180804892938,-0.76769619274218));
#12816=CARTESIAN_POINT('Ctrl Pts',(-13.2407555507495,5.0174130007776,-0.672496539421838));
#12817=CARTESIAN_POINT('Ctrl Pts',(-13.1337092699761,5.28919013266817,-0.5713225204076));
#12818=CARTESIAN_POINT('Ctrl Pts',(-12.2765811993519,7.28310027860678,0.218054325189944));
#12819=CARTESIAN_POINT('Ctrl Pts',(-11.1912637350643,8.82730920467356,1.08947071342651));
#12820=CARTESIAN_POINT('Ctrl Pts',(-8.72366651892778,11.2627708665691,2.58238150810522));
#12821=CARTESIAN_POINT('Ctrl Pts',(-7.16749797466001,12.3407141939304,3.32439961684678));
#12822=CARTESIAN_POINT('Ctrl Pts',(-5.30737084438806,13.1207939135053,3.87257838053821));
#12823=CARTESIAN_POINT('Ctrl Pts',(-5.19427083564474,13.1665430298075,3.90479457078127));
#12824=CARTESIAN_POINT('Ctrl Pts',(-5.08045717850761,13.2108968966417,3.93608070944324));
#12825=CARTESIAN_POINT('',(-13.2173018321168,4.74181238705812,5.83229180537995));
#12826=CARTESIAN_POINT('Ctrl Pts',(-13.339490057964,4.74181238705812,-0.767702284898452));
#12827=CARTESIAN_POINT('Ctrl Pts',(-13.2781486012827,4.74181238705812,2.54732423788973));
#12828=CARTESIAN_POINT('Ctrl Pts',(-13.2173018321188,4.74181238705812,5.83229180540079));
#12829=CARTESIAN_POINT('',(-13.1291325405826,-4.98245867427902,5.83229180537995));
#12830=CARTESIAN_POINT('Origin',(0.135922068665986,0.000349899298694283,
5.83229180537995));
#12831=CARTESIAN_POINT('Ctrl Pts',(-13.1291325405826,-4.98245867427902,
5.83229180537995));
#12832=CARTESIAN_POINT('Ctrl Pts',(-13.1493356074637,-4.98245867427902,
4.74877968014184));
#12833=CARTESIAN_POINT('Ctrl Pts',(-13.1898154199253,-4.98245867427902,
2.57719051924169));
#12834=CARTESIAN_POINT('Ctrl Pts',(-13.2302726269444,-4.98245867427902,
0.405600937068007));
#12835=CARTESIAN_POINT('Ctrl Pts',(-13.2505381529841,-4.98245867427902,
-0.68247630754827));
#12836=CARTESIAN_POINT('Origin',(-13.5749885148034,2.62967685638955,-4.46806532836687));
#12837=CARTESIAN_POINT('',(-16.497528189245,-2.87032314361045,-1.54552565392526));
#12838=CARTESIAN_POINT('',(-13.5749885148034,-2.87032314361045,-4.46806532836687));
#12839=CARTESIAN_POINT('',(-16.497528189245,2.62967685638955,-1.54552565392526));
#12840=CARTESIAN_POINT('Origin',(-21.3531631078554,-2.87032314361045,-12.2462399214189));
#12841=CARTESIAN_POINT('',(-14.9418932706346,-2.87032314361045,-1.54552565392526));
#12842=CARTESIAN_POINT('',(-19.6087980264659,-2.87032314361045,-6.21243040975647));
#12843=CARTESIAN_POINT('Origin',(-15.7197107299398,-2.87032314361045,-0.767708194620052));
#12844=CARTESIAN_POINT('Origin',(-21.3531631078554,2.62967685638955,-12.2462399214189));
#12845=CARTESIAN_POINT('',(-16.497528189245,2.62967685638955,-1.54552565392526));
#12846=CARTESIAN_POINT('',(-13.5749885148034,2.62967685638955,-4.46806532836687));
#12847=CARTESIAN_POINT('',(-14.9418932706346,2.62967685638955,-1.54552565392526));
#12848=CARTESIAN_POINT('',(-19.6087980264659,2.62967685638955,-6.21243040975647));
#12849=CARTESIAN_POINT('Origin',(-15.7197107299398,2.62967685638955,-0.767708194620052));
#12850=CARTESIAN_POINT('Origin',(-12.0361190763098,0.000349899298694283,
-13.7851093599125));
#12851=CARTESIAN_POINT('',(-20.3866154857711,-4.98245867427902,-5.43461295045127));
#12852=CARTESIAN_POINT('',(-22.1309805671606,-4.98245867427902,-3.69024786906167));
#12853=CARTESIAN_POINT('',(-19.6087980264659,-4.98245867427902,-6.21243040975647));
#12854=CARTESIAN_POINT('',(-22.1309805671606,-2.87032314361045,-3.69024786906167));
#12855=CARTESIAN_POINT('',(-22.1309805671606,-2.87032314361045,-3.69024786906167));
#12856=CARTESIAN_POINT('',(-20.3866154857711,-2.87032314361045,-5.43461295045127));
#12857=CARTESIAN_POINT('',(-12.0361190763098,-2.87032314361045,-13.7851093599125));
#12858=CARTESIAN_POINT('',(-20.3866154857711,-4.98245867427902,-5.43461295045127));
#12859=CARTESIAN_POINT('Origin',(0.135922068665986,0.000349899298694283,
-1.61306821493671));
#12860=CARTESIAN_POINT('',(-13.3395039193314,-4.74107350453719,-0.767708194620046));
#12861=CARTESIAN_POINT('Origin',(0.135922068665986,0.000349899298694283,
-0.767708194620051));
#12862=CARTESIAN_POINT('Ctrl Pts',(-13.3395039193314,-4.74107350453718,
-0.767708194620051));
#12863=CARTESIAN_POINT('Ctrl Pts',(-13.5595899825791,-4.12673469180454,
-0.979912166561785));
#12864=CARTESIAN_POINT('Ctrl Pts',(-13.7382816024804,-3.49326423992937,
-1.16221207358175));
#12865=CARTESIAN_POINT('Ctrl Pts',(-14.0655382696254,-1.91389512029188,
-1.50346894589392));
#12866=CARTESIAN_POINT('Ctrl Pts',(-14.164077931334,-0.954643474757865,
-1.61306821493671));
#12867=CARTESIAN_POINT('Ctrl Pts',(-14.164077931334,0.955343273355252,-1.61306821493671));
#12868=CARTESIAN_POINT('Ctrl Pts',(-14.0655382696254,1.91459491888927,-1.50346894589392));
#12869=CARTESIAN_POINT('Ctrl Pts',(-13.7382816024804,3.49396403852676,-1.16221207358175));
#12870=CARTESIAN_POINT('Ctrl Pts',(-13.5595899825791,4.12743449040194,-0.979912166561781));
#12871=CARTESIAN_POINT('Ctrl Pts',(-13.3395039193314,4.74177330313459,-0.767708194620044));
#12872=CARTESIAN_POINT('Origin',(0.0218920916114575,39.6003498992987,-14.6253990787018));
#12873=CARTESIAN_POINT('',(-8.66407793133402,-8.24965010070131,2.55355388009327));
#12874=CARTESIAN_POINT('',(-5.0804571785076,-8.24965010070131,3.93608070944324));
#12875=CARTESIAN_POINT('Origin',(0.0218920916114575,-8.24965010070131,-14.6253990787018));
#12876=CARTESIAN_POINT('',(-5.0804571785076,39.6003498992987,3.93608070944324));
#12877=CARTESIAN_POINT('Origin',(-3.56182917946212,1.09754136743265,5.99267018676129));
#12878=CARTESIAN_POINT('',(-5.0804571785076,8.25034989929869,3.93608070944324));
#12879=CARTESIAN_POINT('',(-5.0804571785076,39.6003498992987,3.93608070944324));
#12880=CARTESIAN_POINT('',(-8.66407793133402,8.25034989929869,2.55355388009326));
#12881=CARTESIAN_POINT('Origin',(0.0218920916114575,8.2503498992987,-14.6253990787018));
#12882=CARTESIAN_POINT('',(-8.66407793133402,39.6003498992987,2.55355388009327));
#12883=CARTESIAN_POINT('Origin',(14.2061209221522,39.6003498992987,-1.45654689569859));
#12884=CARTESIAN_POINT('',(13.9997902889911,-17.,17.0911694938297));
#12885=CARTESIAN_POINT('',(13.9019434616744,0.000349899298694283,25.8869317850633));
#12886=CARTESIAN_POINT('Origin',(0.135922068665986,0.000349899298694283,
25.8869317850633));
#12887=CARTESIAN_POINT('Origin',(17.735922068666,-8.24965010070131,-16.9581329720854));
#12888=CARTESIAN_POINT('',(-0.11761019287632,-8.24965010070131,7.09490065582709));
#12889=CARTESIAN_POINT('',(7.42524145690086,-8.24965010070131,13.731996542212));
#12890=CARTESIAN_POINT('Origin',(26.5767111010661,-8.24965010070131,-15.6377043248233));
#12891=CARTESIAN_POINT('Origin',(-7.7310282279201,-8.24965010070131,13.578407872116));
#12892=CARTESIAN_POINT('',(-8.66407793133402,-8.24965010070131,21.731996542212));
#12893=CARTESIAN_POINT('',(-8.66407793133402,-8.24965010070131,-16.9581329720854));
#12894=CARTESIAN_POINT('',(7.42524145690086,-8.24965010070131,21.731996542212));
#12895=CARTESIAN_POINT('',(7.42524145690086,-8.24965010070131,21.731996542212));
#12896=CARTESIAN_POINT('',(7.42524145690086,-8.24965010070131,21.731996542212));
#12897=CARTESIAN_POINT('Origin',(17.735922068666,8.2503498992987,-16.9581329720854));
#12898=CARTESIAN_POINT('',(-0.11761019287632,8.25034989929869,7.09490065582709));
#12899=CARTESIAN_POINT('Origin',(-7.7310282279201,8.25034989929869,13.578407872116));
#12900=CARTESIAN_POINT('',(7.42524145690086,8.25034989929869,13.731996542212));
#12901=CARTESIAN_POINT('Origin',(26.5767111010661,8.2503498992987,-15.6377043248233));
#12902=CARTESIAN_POINT('',(7.42524145690086,8.25034989929869,21.731996542212));
#12903=CARTESIAN_POINT('',(7.42524145690086,8.25034989929869,21.731996542212));
#12904=CARTESIAN_POINT('',(-8.66407793133402,8.25034989929869,21.731996542212));
#12905=CARTESIAN_POINT('',(-8.66407793133402,8.25034989929869,21.731996542212));
#12906=CARTESIAN_POINT('',(-8.66407793133402,8.2503498992987,-16.9581329720854));
#12907=CARTESIAN_POINT('Origin',(-8.66407793133402,0.000349899298694283,
-1.61306821493671));
#12908=CARTESIAN_POINT('',(-8.66407793133402,-8.24965010070131,21.731996542212));
#12909=CARTESIAN_POINT('Origin',(14.2231693005462,-4.98245867427902,-0.767708194620051));
#12910=CARTESIAN_POINT('',(-13.2521255922709,-4.98245867427902,-0.767708194620051));
#12911=CARTESIAN_POINT('Origin',(0.135922068665986,0.000349899298694283,
-0.767708194620051));
#12912=CARTESIAN_POINT('',(-14.1640758113294,-4.98245867427902,-0.76770819462005));
#12913=CARTESIAN_POINT('',(14.2231693005462,-4.98245867427902,-0.767708194620051));
#12914=CARTESIAN_POINT('',(-14.1640758113294,4.74181238705812,-0.767708194620056));
#12915=CARTESIAN_POINT('',(-14.1640758113294,-4.98245867427902,-0.767708194620051));
#12916=CARTESIAN_POINT('',(14.2231693005462,4.74181238705812,-0.767708194620051));
#12917=CARTESIAN_POINT('Origin',(14.2231693005462,4.74181238705812,5.83229180537995));
#12918=CARTESIAN_POINT('',(-22.1309805671606,4.74181238705812,-3.69024786906167));
#12919=CARTESIAN_POINT('',(-20.386615485771,4.74181238705812,-5.43461295045127));
#12920=CARTESIAN_POINT('',(-22.9087980264659,4.74181238705812,-2.91243040975647));
#12921=CARTESIAN_POINT('',(-22.1309805671606,4.74181238705812,-2.13461295045127));
#12922=CARTESIAN_POINT('Origin',(-21.3531631078554,4.74181238705812,-2.91243040975647));
#12923=CARTESIAN_POINT('',(-14.1640758113294,4.74181238705812,5.83229180537995));
#12924=CARTESIAN_POINT('',(-22.9087980264659,4.74181238705812,-2.91243040975647));
#12925=CARTESIAN_POINT('',(14.2231693005462,4.74181238705812,5.83229180537995));
#12926=CARTESIAN_POINT('',(-18.8309805671606,4.74181238705812,-5.43461295045127));
#12927=CARTESIAN_POINT('',(-19.6087980264659,4.74181238705812,-6.21243040975647));
#12928=CARTESIAN_POINT('Origin',(-19.6087980264659,4.74181238705812,-4.65679549114606));
#12929=CARTESIAN_POINT('Origin',(14.2231693005462,-4.98245867427902,5.83229180537995));
#12930=CARTESIAN_POINT('',(-14.1640758113294,-4.98245867427902,5.83229180537995));
#12931=CARTESIAN_POINT('',(-14.1640758113294,-4.98245867427902,5.83229180537995));
#12932=CARTESIAN_POINT('',(14.2231693005462,-4.98245867427902,5.83229180537995));
#12933=CARTESIAN_POINT('Origin',(14.2231693005462,-4.98245867427902,5.83229180537995));
#12934=CARTESIAN_POINT('',(-22.1309805671606,-4.98245867427902,-2.13461295045127));
#12935=CARTESIAN_POINT('',(-22.9087980264659,-4.98245867427902,-2.91243040975647));
#12936=CARTESIAN_POINT('Origin',(-21.3531631078554,-4.98245867427902,-2.91243040975647));
#12937=CARTESIAN_POINT('',(-18.8309805671606,-4.98245867427902,-5.43461295045127));
#12938=CARTESIAN_POINT('Origin',(-19.6087980264659,-4.98245867427902,-4.65679549114606));
#12939=CARTESIAN_POINT('',(-19.6087980264659,-4.98245867427902,-6.21243040975647));
#12940=CARTESIAN_POINT('',(-13.2505381529841,-4.98245867427902,-0.68247630754827));
#12941=CARTESIAN_POINT('Origin',(0.135922068665986,0.000349899298694283,
-1.61306821493671));
#12942=CARTESIAN_POINT('Origin',(-19.6087980264659,4.74181238705812,-6.21243040975647));
#12943=CARTESIAN_POINT('',(-18.8309805671606,2.62967685638955,-5.43461295045127));
#12944=CARTESIAN_POINT('',(-19.6087980264659,2.62967685638955,-6.21243040975647));
#12945=CARTESIAN_POINT('',(-18.8309805671606,4.74181238705812,-5.43461295045127));
#12946=CARTESIAN_POINT('',(-18.8309805671606,-2.87032314361045,-5.43461295045127));
#12947=CARTESIAN_POINT('',(-18.8309805671606,-2.87032314361045,-5.43461295045127));
#12948=CARTESIAN_POINT('',(-19.6087980264659,-2.87032314361045,-6.21243040975647));
#12949=CARTESIAN_POINT('',(-14.9418932706346,4.74181238705812,-1.54552565392526));
#12950=CARTESIAN_POINT('Origin',(-22.9087980264659,-4.98245867427902,-2.91243040975647));
#12951=CARTESIAN_POINT('',(-22.1309805671606,2.62967685638955,-2.13461295045127));
#12952=CARTESIAN_POINT('',(-26.7978853229919,2.62967685638955,-6.80151770628248));
#12953=CARTESIAN_POINT('',(-22.1309805671606,-2.87032314361045,-2.13461295045127));
#12954=CARTESIAN_POINT('',(-26.7978853229919,-2.87032314361045,-6.80151770628248));
#12955=CARTESIAN_POINT('',(-22.1309805671606,-4.98245867427902,-2.13461295045127));
#12956=CARTESIAN_POINT('',(-22.1309805671606,2.62967685638955,-2.13461295045127));
#12957=CARTESIAN_POINT('Origin',(-12.0361190763098,0.000349899298694283,
-13.7851093599125));
#12958=CARTESIAN_POINT('',(-22.1309805671606,2.62967685638955,-3.69024786906167));
#12959=CARTESIAN_POINT('',(-20.3866154857711,2.62967685638955,-5.43461295045127));
#12960=CARTESIAN_POINT('',(-12.0361190763098,2.62967685638955,-13.7851093599125));
#12961=CARTESIAN_POINT('',(-22.1309805671606,4.74181238705812,-3.69024786906167));
#12962=CARTESIAN_POINT('',(-20.3866154857711,2.62967685638955,-5.43461295045127));
#12963=CARTESIAN_POINT('Origin',(-13.5749885148034,2.62967685638955,-4.46806532836687));
#12964=CARTESIAN_POINT('',(-16.497528189245,2.62967685638955,-1.54552565392526));
#12965=CARTESIAN_POINT('Origin',(-21.3531631078554,-2.87032314361045,-12.2462399214189));
#12966=CARTESIAN_POINT('Origin',(-19.6087980264659,-2.87032314361045,-4.65679549114606));
#12967=CARTESIAN_POINT('Origin',(-21.3531631078554,-2.87032314361045,-2.91243040975647));
#12968=CARTESIAN_POINT('Origin',(-21.3531631078554,2.62967685638955,-12.2462399214189));
#12969=CARTESIAN_POINT('Origin',(-21.3531631078554,2.62967685638955,-2.91243040975647));
#12970=CARTESIAN_POINT('Origin',(-19.6087980264659,2.62967685638955,-4.65679549114606));
#12971=CARTESIAN_POINT('Origin',(-19.7031631078554,-6.08245867427902,-3.00679549114607));
#12972=CARTESIAN_POINT('Origin',(-19.7031631078554,5.84154132572098,-3.00679549114607));
#12973=CARTESIAN_POINT('Origin',(-21.3531631078554,0.000349899298694283,
-2.91243040975647));
#12974=CARTESIAN_POINT('Origin',(-21.3531631078554,0.000349899298694283,
-2.91243040975647));
#12975=CARTESIAN_POINT('Origin',(-19.6087980264659,0.000349899298694283,
-4.65679549114606));
#12976=CARTESIAN_POINT('Origin',(-19.6087980264659,0.000349899298694283,
-4.65679549114606));
#12977=CARTESIAN_POINT('Origin',(-15.7197107299398,4.74181238705812,-0.767708194620052));
#12978=CARTESIAN_POINT('Origin',(26.5767111010661,-17.,-15.6377043248233));
#12979=CARTESIAN_POINT('',(-0.11761019287632,-17.,7.09490065582709));
#12980=CARTESIAN_POINT('',(7.42524145690086,-17.,13.731996542212));
#12981=CARTESIAN_POINT('',(-0.11761019287632,-17.,7.09490065582709));
#12982=CARTESIAN_POINT('Origin',(7.42524145690086,8.25034989929869,21.731996542212));
#12983=CARTESIAN_POINT('',(7.42524145690086,8.25034989929869,21.731996542212));
#12984=CARTESIAN_POINT('Origin',(-6.22633625589568E-31,-3.81260606886127E-15,
21.731996542212));
#12985=CARTESIAN_POINT('Origin',(-7.7310282279201,39.6003498992987,13.578407872116));
#12986=CARTESIAN_POINT('Origin',(-7.7310282279201,39.6003498992987,13.578407872116));
#12987=CARTESIAN_POINT('',(0.,0.,0.));
#12988=CARTESIAN_POINT('Ctrl Pts',(0.,22.9756202217091,1.38777878078145E-15));
#12989=CARTESIAN_POINT('Ctrl Pts',(-1.38777878078145E-15,22.9756202217091,
1.38777878078145E-15));
#12990=CARTESIAN_POINT('Ctrl Pts',(-1.38777878078145E-15,22.9756202217091,
0.));
#12991=CARTESIAN_POINT('Ctrl Pts',(-1.38777878078145E-15,22.9756202217091,
-1.38777878078145E-15));
#12992=CARTESIAN_POINT('Ctrl Pts',(0.,22.9756202217091,-1.38777878078145E-15));
#12993=CARTESIAN_POINT('Ctrl Pts',(1.38777878078145E-15,22.9756202217091,
-1.38777878078145E-15));
#12994=CARTESIAN_POINT('Ctrl Pts',(1.38777878078145E-15,22.9756202217091,
0.));
#12995=CARTESIAN_POINT('Ctrl Pts',(1.38777878078145E-15,22.9756202217091,
1.38777878078145E-15));
#12996=CARTESIAN_POINT('Ctrl Pts',(0.,22.9756202217091,1.38777878078145E-15));
#12997=CARTESIAN_POINT('Ctrl Pts',(0.,22.3010873717989,7.46986335401695));
#12998=CARTESIAN_POINT('Ctrl Pts',(-7.46986335401695,22.3010873717989,7.46986335401695));
#12999=CARTESIAN_POINT('Ctrl Pts',(-7.46986335401695,22.3010873717989,0.));
#13000=CARTESIAN_POINT('Ctrl Pts',(-7.46986335401695,22.3010873717989,-7.46986335401695));
#13001=CARTESIAN_POINT('Ctrl Pts',(0.,22.3010873717989,-7.46986335401695));
#13002=CARTESIAN_POINT('Ctrl Pts',(7.46986335401695,22.3010873717989,-7.46986335401695));
#13003=CARTESIAN_POINT('Ctrl Pts',(7.46986335401695,22.3010873717989,0.));
#13004=CARTESIAN_POINT('Ctrl Pts',(7.46986335401695,22.3010873717989,7.46986335401695));
#13005=CARTESIAN_POINT('Ctrl Pts',(0.,22.3010873717989,7.46986335401695));
#13006=CARTESIAN_POINT('Ctrl Pts',(0.,15.6086878860909,10.8559587775082));
#13007=CARTESIAN_POINT('Ctrl Pts',(-10.8559587775082,15.6086878860909,10.8559587775082));
#13008=CARTESIAN_POINT('Ctrl Pts',(-10.8559587775082,15.6086878860909,0.));
#13009=CARTESIAN_POINT('Ctrl Pts',(-10.8559587775082,15.6086878860909,-10.8559587775082));
#13010=CARTESIAN_POINT('Ctrl Pts',(0.,15.6086878860909,-10.8559587775082));
#13011=CARTESIAN_POINT('Ctrl Pts',(10.8559587775082,15.6086878860909,-10.8559587775082));
#13012=CARTESIAN_POINT('Ctrl Pts',(10.8559587775082,15.6086878860909,0.));
#13013=CARTESIAN_POINT('Ctrl Pts',(10.8559587775082,15.6086878860909,10.8559587775082));
#13014=CARTESIAN_POINT('Ctrl Pts',(0.,15.6086878860909,10.8559587775082));
#13015=CARTESIAN_POINT('',(1.51096669663837E-15,15.6086878860909,10.8559587775082));
#13016=CARTESIAN_POINT('Origin',(0.,15.6086878860909,0.));
#13017=CARTESIAN_POINT('',(1.30104260698261E-15,22.9756202217091,0.));
#13018=CARTESIAN_POINT('Origin',(1.49018292596266E-16,9.50032514580282,
-1.21682670219706));
#13019=CARTESIAN_POINT('Ctrl Pts',(0.,15.6086878860909,10.8559587775082));
#13020=CARTESIAN_POINT('Ctrl Pts',(-10.8559587775082,15.6086878860909,10.8559587775082));
#13021=CARTESIAN_POINT('Ctrl Pts',(-10.8559587775082,15.6086878860909,0.));
#13022=CARTESIAN_POINT('Ctrl Pts',(-10.8559587775082,15.6086878860909,-10.8559587775082));
#13023=CARTESIAN_POINT('Ctrl Pts',(0.,15.6086878860909,-10.8559587775082));
#13024=CARTESIAN_POINT('Ctrl Pts',(10.8559587775082,15.6086878860909,-10.8559587775082));
#13025=CARTESIAN_POINT('Ctrl Pts',(10.8559587775082,15.6086878860909,0.));
#13026=CARTESIAN_POINT('Ctrl Pts',(10.8559587775082,15.6086878860909,10.8559587775082));
#13027=CARTESIAN_POINT('Ctrl Pts',(0.,15.6086878860909,10.8559587775082));
#13028=CARTESIAN_POINT('Ctrl Pts',(0.,8.06226657049109,13.6962040180237));
#13029=CARTESIAN_POINT('Ctrl Pts',(-13.6962040180237,8.06226657049109,13.6962040180237));
#13030=CARTESIAN_POINT('Ctrl Pts',(-13.6962040180237,8.06226657049109,0.));
#13031=CARTESIAN_POINT('Ctrl Pts',(-13.6962040180237,8.06226657049109,-13.6962040180237));
#13032=CARTESIAN_POINT('Ctrl Pts',(0.,8.06226657049109,-13.6962040180237));
#13033=CARTESIAN_POINT('Ctrl Pts',(13.6962040180237,8.06226657049109,-13.6962040180237));
#13034=CARTESIAN_POINT('Ctrl Pts',(13.6962040180237,8.06226657049109,0.));
#13035=CARTESIAN_POINT('Ctrl Pts',(13.6962040180237,8.06226657049109,13.6962040180237));
#13036=CARTESIAN_POINT('Ctrl Pts',(0.,8.06226657049109,13.6962040180237));
#13037=CARTESIAN_POINT('Ctrl Pts',(0.,0.,13.82));
#13038=CARTESIAN_POINT('Ctrl Pts',(-13.82,0.,13.82));
#13039=CARTESIAN_POINT('Ctrl Pts',(-13.82,0.,0.));
#13040=CARTESIAN_POINT('Ctrl Pts',(-13.82,0.,-13.82));
#13041=CARTESIAN_POINT('Ctrl Pts',(0.,0.,-13.82));
#13042=CARTESIAN_POINT('Ctrl Pts',(13.82,0.,-13.82));
#13043=CARTESIAN_POINT('Ctrl Pts',(13.82,0.,0.));
#13044=CARTESIAN_POINT('Ctrl Pts',(13.82,0.,13.82));
#13045=CARTESIAN_POINT('Ctrl Pts',(0.,0.,13.82));
#13046=CARTESIAN_POINT('',(-1.69246187642164E-15,0.,13.82));
#13047=CARTESIAN_POINT('Origin',(0.,0.,0.));
#13048=CARTESIAN_POINT('Origin',(3.98079965616974E-15,-0.711330365603759,
-32.505696001013));
#13049=CARTESIAN_POINT('Origin',(0.,0.,0.));
#13050=CARTESIAN_POINT('',(0.,0.,0.));
#13051=CARTESIAN_POINT('',(0.,0.,0.));
#13052=CARTESIAN_POINT('Origin',(3.77881193895716E-17,0.,11.9128278522764));
#13053=CARTESIAN_POINT('',(-2.,-2.44929359829471E-16,11.9128278522764));
#13054=CARTESIAN_POINT('Origin',(3.77881193895716E-17,0.,11.9128278522764));
#13055=CARTESIAN_POINT('',(-2.,-2.44929359829471E-16,33.5128278522764));
#13056=CARTESIAN_POINT('',(-2.,-2.44929359829471E-16,11.9128278522764));
#13057=CARTESIAN_POINT('Origin',(3.77881193895716E-17,0.,33.5128278522764));
#13058=CARTESIAN_POINT('Origin',(-3.2,4.19224840027728E-16,0.712827852276406));
#13059=CARTESIAN_POINT('',(-1.6,-1.2,0.712827852276406));
#13060=CARTESIAN_POINT('Origin',(-1.6,2.45752492430048E-16,0.712827852276406));
#13061=CARTESIAN_POINT('',(1.6,-1.2,0.712827852276406));
#13062=CARTESIAN_POINT('',(-3.2,-1.2,0.712827852276406));
#13063=CARTESIAN_POINT('Origin',(1.6,-1.01192202765314E-16,0.712827852276406));
#13064=CARTESIAN_POINT('Origin',(3.77881193895716E-17,0.,33.5128278522764));
#13065=CARTESIAN_POINT('',(3.2,-3.91886975727153E-16,3.11282785227641));
#13066=CARTESIAN_POINT('Origin',(3.77881193895716E-17,0.,3.11282785227641));
#13067=CARTESIAN_POINT('',(3.2,-3.91886975727153E-16,33.5128278522764));
#13068=CARTESIAN_POINT('',(3.2,-3.91886975727153E-16,33.5128278522764));
#13069=CARTESIAN_POINT('Origin',(3.77881193895716E-17,0.,33.5128278522764));
#13070=CARTESIAN_POINT('Origin',(3.77881193895716E-17,0.,3.11282785227641));
#13071=CARTESIAN_POINT('',(-1.6,-2.4,3.11282785227641));
#13072=CARTESIAN_POINT('',(-1.6,2.4,3.11282785227641));
#13073=CARTESIAN_POINT('',(-1.6,2.4,3.11282785227641));
#13074=CARTESIAN_POINT('',(1.6,-2.4,3.11282785227641));
#13075=CARTESIAN_POINT('',(1.6,-2.4,3.11282785227641));
#13076=CARTESIAN_POINT('',(1.6,2.4,3.11282785227641));
#13077=CARTESIAN_POINT('',(1.6,2.4,3.11282785227641));
#13078=CARTESIAN_POINT('',(1.6,2.4,3.11282785227641));
#13079=CARTESIAN_POINT('Origin',(3.77881193895716E-17,0.,33.5128278522764));
#13080=CARTESIAN_POINT('Origin',(-1.6,2.4,-1.68717214772359));
#13081=CARTESIAN_POINT('',(-1.6,2.4,0.712827852276406));
#13082=CARTESIAN_POINT('',(-1.6,-2.4,0.712827852276406));
#13083=CARTESIAN_POINT('Origin',(-1.6,0.,0.712827852276406));
#13084=CARTESIAN_POINT('',(-1.6,-2.4,-1.68717214772359));
#13085=CARTESIAN_POINT('',(-1.6,2.4,-1.68717214772359));
#13086=CARTESIAN_POINT('Origin',(1.6,2.4,-1.68717214772359));
#13087=CARTESIAN_POINT('',(1.6,2.4,0.712827852276406));
#13088=CARTESIAN_POINT('',(1.6,2.4,-1.68717214772359));
#13089=CARTESIAN_POINT('',(-1.6,2.4,0.712827852276406));
#13090=CARTESIAN_POINT('Origin',(1.6,2.4,-1.68717214772359));
#13091=CARTESIAN_POINT('',(1.6,-2.4,0.712827852276406));
#13092=CARTESIAN_POINT('',(1.6,-2.4,-1.68717214772359));
#13093=CARTESIAN_POINT('Origin',(1.6,0.,0.712827852276406));
#13094=CARTESIAN_POINT('Origin',(1.6,-2.4,-1.68717214772359));
#13095=CARTESIAN_POINT('',(1.6,-2.4,0.712827852276406));
#13096=CARTESIAN_POINT('Origin',(3.77881193895716E-17,0.,0.712827852276406));
#13097=CARTESIAN_POINT('Origin',(3.77881193895716E-17,0.,11.9128278522764));
#13098=CARTESIAN_POINT('',(0.,0.,0.));
#13099=CARTESIAN_POINT('Origin',(-0.8,-8.82901007224409E-16,29.92));
#13100=CARTESIAN_POINT('',(-0.8,-0.799999999999999,29.92));
#13101=CARTESIAN_POINT('Origin',(-0.8,-8.82901007224409E-16,29.92));
#13102=CARTESIAN_POINT('',(0.8,-0.799999999999999,29.92));
#13103=CARTESIAN_POINT('',(-0.8,-0.799999999999999,29.92));
#13104=CARTESIAN_POINT('Origin',(0.8,-6.84646895684203E-16,29.92));
#13105=CARTESIAN_POINT('Origin',(-5.32548339959391,-1.44364831389719E-15,
29.92));
#13106=CARTESIAN_POINT('',(-0.8,-1.4,29.1454033307585));
#13107=CARTESIAN_POINT('',(-0.8,1.4,29.1454033307585));
#13108=CARTESIAN_POINT('Origin',(-0.8,-8.82901007224409E-16,29.92));
#13109=CARTESIAN_POINT('',(0.8,-1.4,29.1454033307585));
#13110=CARTESIAN_POINT('',(-5.32548339959391,-1.4,29.1454033307585));
#13111=CARTESIAN_POINT('',(0.8,1.4,29.1454033307585));
#13112=CARTESIAN_POINT('Origin',(0.8,-6.84646895684203E-16,29.92));
#13113=CARTESIAN_POINT('',(-5.32548339959391,1.4,29.1454033307585));
#13114=CARTESIAN_POINT('Origin',(0.,0.,26.4));
#13115=CARTESIAN_POINT('',(2.,-2.44929359829471E-16,0.));
#13116=CARTESIAN_POINT('Origin',(0.,0.,0.));
#13117=CARTESIAN_POINT('',(2.,-2.44929359829471E-16,26.4));
#13118=CARTESIAN_POINT('',(2.,-2.44929359829471E-16,26.4));
#13119=CARTESIAN_POINT('Origin',(0.,0.,26.4));
#13120=CARTESIAN_POINT('Origin',(0.,0.,26.4));
#13121=CARTESIAN_POINT('',(0.8,1.4,26.4));
#13122=CARTESIAN_POINT('',(-0.8,1.4,26.4));
#13123=CARTESIAN_POINT('',(-0.8,1.4,26.4));
#13124=CARTESIAN_POINT('',(0.8,-1.4,26.4));
#13125=CARTESIAN_POINT('',(0.8,1.4,26.4));
#13126=CARTESIAN_POINT('',(-0.8,-1.4,26.4));
#13127=CARTESIAN_POINT('',(-0.8,-1.4,26.4));
#13128=CARTESIAN_POINT('',(-0.8,1.4,26.4));
#13129=CARTESIAN_POINT('Origin',(0.,0.,0.));
#13130=CARTESIAN_POINT('Origin',(0.8,1.4,29.92));
#13131=CARTESIAN_POINT('',(0.8,1.4,29.92));
#13132=CARTESIAN_POINT('',(0.8,-1.4,29.92));
#13133=CARTESIAN_POINT('Origin',(-0.8,1.4,29.92));
#13134=CARTESIAN_POINT('',(-0.8,1.4,29.92));
#13135=CARTESIAN_POINT('Origin',(-0.8,1.4,29.92));
#13136=CARTESIAN_POINT('',(-0.8,-1.4,29.92));
#13137=CARTESIAN_POINT('Origin',(-0.8,-1.4,29.92));
#13138=CARTESIAN_POINT('',(-13.1648862463908,-2.12457642057909,-6.69250946692211));
#13139=CARTESIAN_POINT('',(-13.1648862463908,-2.1245764205791,18.4203183853543));
#13140=CARTESIAN_POINT('',(10.6052056412698,-21.7821147123702,46.7113807520409));
#13141=CARTESIAN_POINT('',(-1.87678054515791,-4.25756393049714,46.7170487466427));
#13142=CARTESIAN_POINT('',(-29.0919028904004,4.49091910115092,48.7364360961644));
#13143=CARTESIAN_POINT('',(-43.5037524187485,-16.4626543804805,43.8992815919311));
#13144=CARTESIAN_POINT('',(4.63195925578279,17.1877311358157,62.7445614180609));
#13145=CARTESIAN_POINT('',(-25.,15.,32.));
#13146=CARTESIAN_POINT('',(13.3067398065921,84.0077429696187,14.1799263771933));
#13147=CARTESIAN_POINT('',(-5.59905124923421,82.0609881837313,40.3069128102954));
#13148=UNCERTAINTY_MEASURE_WITH_UNIT(LENGTH_MEASURE(0.01),#13200,
'DISTANCE_ACCURACY_VALUE',
'Maximum model space distance between geometric entities at asserted c
onnectivities');
#13149=UNCERTAINTY_MEASURE_WITH_UNIT(LENGTH_MEASURE(0.01),#13200,
'DISTANCE_ACCURACY_VALUE',
'Maximum model space distance between geometric entities at asserted c
onnectivities');
#13150=UNCERTAINTY_MEASURE_WITH_UNIT(LENGTH_MEASURE(0.01),#13200,
'DISTANCE_ACCURACY_VALUE',
'Maximum model space distance between geometric entities at asserted c
onnectivities');
#13151=UNCERTAINTY_MEASURE_WITH_UNIT(LENGTH_MEASURE(0.01),#13200,
'DISTANCE_ACCURACY_VALUE',
'Maximum model space distance between geometric entities at asserted c
onnectivities');
#13152=UNCERTAINTY_MEASURE_WITH_UNIT(LENGTH_MEASURE(0.01),#13200,
'DISTANCE_ACCURACY_VALUE',
'Maximum model space distance between geometric entities at asserted c
onnectivities');
#13153=UNCERTAINTY_MEASURE_WITH_UNIT(LENGTH_MEASURE(0.01),#13200,
'DISTANCE_ACCURACY_VALUE',
'Maximum model space distance between geometric entities at asserted c
onnectivities');
#13154=UNCERTAINTY_MEASURE_WITH_UNIT(LENGTH_MEASURE(0.01),#13200,
'DISTANCE_ACCURACY_VALUE',
'Maximum model space distance between geometric entities at asserted c
onnectivities');
#13155=UNCERTAINTY_MEASURE_WITH_UNIT(LENGTH_MEASURE(0.01),#13200,
'DISTANCE_ACCURACY_VALUE',
'Maximum model space distance between geometric entities at asserted c
onnectivities');
#13156=UNCERTAINTY_MEASURE_WITH_UNIT(LENGTH_MEASURE(0.01),#13200,
'DISTANCE_ACCURACY_VALUE',
'Maximum model space distance between geometric entities at asserted c
onnectivities');
#13157=UNCERTAINTY_MEASURE_WITH_UNIT(LENGTH_MEASURE(0.01),#13200,
'DISTANCE_ACCURACY_VALUE',
'Maximum model space distance between geometric entities at asserted c
onnectivities');
#13158=UNCERTAINTY_MEASURE_WITH_UNIT(LENGTH_MEASURE(0.01),#13200,
'DISTANCE_ACCURACY_VALUE',
'Maximum model space distance between geometric entities at asserted c
onnectivities');
#13159=UNCERTAINTY_MEASURE_WITH_UNIT(LENGTH_MEASURE(0.01),#13200,
'DISTANCE_ACCURACY_VALUE',
'Maximum model space distance between geometric entities at asserted c
onnectivities');
#13160=UNCERTAINTY_MEASURE_WITH_UNIT(LENGTH_MEASURE(0.01),#13200,
'DISTANCE_ACCURACY_VALUE',
'Maximum model space distance between geometric entities at asserted c
onnectivities');
#13161=UNCERTAINTY_MEASURE_WITH_UNIT(LENGTH_MEASURE(0.01),#13200,
'DISTANCE_ACCURACY_VALUE',
'Maximum model space distance between geometric entities at asserted c
onnectivities');
#13162=UNCERTAINTY_MEASURE_WITH_UNIT(LENGTH_MEASURE(0.01),#13200,
'DISTANCE_ACCURACY_VALUE',
'Maximum model space distance between geometric entities at asserted c
onnectivities');
#13163=UNCERTAINTY_MEASURE_WITH_UNIT(LENGTH_MEASURE(0.01),#13200,
'DISTANCE_ACCURACY_VALUE',
'Maximum model space distance between geometric entities at asserted c
onnectivities');
#13164=UNCERTAINTY_MEASURE_WITH_UNIT(LENGTH_MEASURE(0.01),#13200,
'DISTANCE_ACCURACY_VALUE',
'Maximum model space distance between geometric entities at asserted c
onnectivities');
#13165=UNCERTAINTY_MEASURE_WITH_UNIT(LENGTH_MEASURE(0.01),#13200,
'DISTANCE_ACCURACY_VALUE',
'Maximum model space distance between geometric entities at asserted c
onnectivities');
#13166=UNCERTAINTY_MEASURE_WITH_UNIT(LENGTH_MEASURE(0.01),#13200,
'DISTANCE_ACCURACY_VALUE',
'Maximum model space distance between geometric entities at asserted c
onnectivities');
#13167=UNCERTAINTY_MEASURE_WITH_UNIT(LENGTH_MEASURE(0.01),#13200,
'DISTANCE_ACCURACY_VALUE',
'Maximum model space distance between geometric entities at asserted c
onnectivities');
#13168=UNCERTAINTY_MEASURE_WITH_UNIT(LENGTH_MEASURE(0.01),#13200,
'DISTANCE_ACCURACY_VALUE',
'Maximum model space distance between geometric entities at asserted c
onnectivities');
#13169=UNCERTAINTY_MEASURE_WITH_UNIT(LENGTH_MEASURE(0.01),#13200,
'DISTANCE_ACCURACY_VALUE',
'Maximum model space distance between geometric entities at asserted c
onnectivities');
#13170=UNCERTAINTY_MEASURE_WITH_UNIT(LENGTH_MEASURE(0.01),#13200,
'DISTANCE_ACCURACY_VALUE',
'Maximum model space distance between geometric entities at asserted c
onnectivities');
#13171=UNCERTAINTY_MEASURE_WITH_UNIT(LENGTH_MEASURE(0.01),#13200,
'DISTANCE_ACCURACY_VALUE',
'Maximum model space distance between geometric entities at asserted c
onnectivities');
#13172=UNCERTAINTY_MEASURE_WITH_UNIT(LENGTH_MEASURE(0.01),#13200,
'DISTANCE_ACCURACY_VALUE',
'Maximum model space distance between geometric entities at asserted c
onnectivities');
#13173=UNCERTAINTY_MEASURE_WITH_UNIT(LENGTH_MEASURE(0.01),#13200,
'DISTANCE_ACCURACY_VALUE',
'Maximum model space distance between geometric entities at asserted c
onnectivities');
#13174=(
GEOMETRIC_REPRESENTATION_CONTEXT(3)
GLOBAL_UNCERTAINTY_ASSIGNED_CONTEXT((#13148))
GLOBAL_UNIT_ASSIGNED_CONTEXT((#13200,#13202,#13203))
REPRESENTATION_CONTEXT('','3D')
);
#13175=(
GEOMETRIC_REPRESENTATION_CONTEXT(3)
GLOBAL_UNCERTAINTY_ASSIGNED_CONTEXT((#13149))
GLOBAL_UNIT_ASSIGNED_CONTEXT((#13200,#13202,#13203))
REPRESENTATION_CONTEXT('','3D')
);
#13176=(
GEOMETRIC_REPRESENTATION_CONTEXT(3)
GLOBAL_UNCERTAINTY_ASSIGNED_CONTEXT((#13150))
GLOBAL_UNIT_ASSIGNED_CONTEXT((#13200,#13202,#13203))
REPRESENTATION_CONTEXT('','3D')
);
#13177=(
GEOMETRIC_REPRESENTATION_CONTEXT(3)
GLOBAL_UNCERTAINTY_ASSIGNED_CONTEXT((#13151))
GLOBAL_UNIT_ASSIGNED_CONTEXT((#13200,#13202,#13203))
REPRESENTATION_CONTEXT('','3D')
);
#13178=(
GEOMETRIC_REPRESENTATION_CONTEXT(3)
GLOBAL_UNCERTAINTY_ASSIGNED_CONTEXT((#13152))
GLOBAL_UNIT_ASSIGNED_CONTEXT((#13200,#13202,#13203))
REPRESENTATION_CONTEXT('','3D')
);
#13179=(
GEOMETRIC_REPRESENTATION_CONTEXT(3)
GLOBAL_UNCERTAINTY_ASSIGNED_CONTEXT((#13153))
GLOBAL_UNIT_ASSIGNED_CONTEXT((#13200,#13202,#13203))
REPRESENTATION_CONTEXT('','3D')
);
#13180=(
GEOMETRIC_REPRESENTATION_CONTEXT(3)
GLOBAL_UNCERTAINTY_ASSIGNED_CONTEXT((#13154))
GLOBAL_UNIT_ASSIGNED_CONTEXT((#13200,#13202,#13203))
REPRESENTATION_CONTEXT('','3D')
);
#13181=(
GEOMETRIC_REPRESENTATION_CONTEXT(3)
GLOBAL_UNCERTAINTY_ASSIGNED_CONTEXT((#13155))
GLOBAL_UNIT_ASSIGNED_CONTEXT((#13200,#13202,#13203))
REPRESENTATION_CONTEXT('','3D')
);
#13182=(
GEOMETRIC_REPRESENTATION_CONTEXT(3)
GLOBAL_UNCERTAINTY_ASSIGNED_CONTEXT((#13156))
GLOBAL_UNIT_ASSIGNED_CONTEXT((#13200,#13202,#13203))
REPRESENTATION_CONTEXT('','3D')
);
#13183=(
GEOMETRIC_REPRESENTATION_CONTEXT(3)
GLOBAL_UNCERTAINTY_ASSIGNED_CONTEXT((#13157))
GLOBAL_UNIT_ASSIGNED_CONTEXT((#13200,#13202,#13203))
REPRESENTATION_CONTEXT('','3D')
);
#13184=(
GEOMETRIC_REPRESENTATION_CONTEXT(3)
GLOBAL_UNCERTAINTY_ASSIGNED_CONTEXT((#13158))
GLOBAL_UNIT_ASSIGNED_CONTEXT((#13200,#13202,#13203))
REPRESENTATION_CONTEXT('','3D')
);
#13185=(
GEOMETRIC_REPRESENTATION_CONTEXT(3)
GLOBAL_UNCERTAINTY_ASSIGNED_CONTEXT((#13159))
GLOBAL_UNIT_ASSIGNED_CONTEXT((#13200,#13202,#13203))
REPRESENTATION_CONTEXT('','3D')
);
#13186=(
GEOMETRIC_REPRESENTATION_CONTEXT(3)
GLOBAL_UNCERTAINTY_ASSIGNED_CONTEXT((#13160))
GLOBAL_UNIT_ASSIGNED_CONTEXT((#13200,#13202,#13203))
REPRESENTATION_CONTEXT('','3D')
);
#13187=(
GEOMETRIC_REPRESENTATION_CONTEXT(3)
GLOBAL_UNCERTAINTY_ASSIGNED_CONTEXT((#13161))
GLOBAL_UNIT_ASSIGNED_CONTEXT((#13200,#13202,#13203))
REPRESENTATION_CONTEXT('','3D')
);
#13188=(
GEOMETRIC_REPRESENTATION_CONTEXT(3)
GLOBAL_UNCERTAINTY_ASSIGNED_CONTEXT((#13162))
GLOBAL_UNIT_ASSIGNED_CONTEXT((#13200,#13202,#13203))
REPRESENTATION_CONTEXT('','3D')
);
#13189=(
GEOMETRIC_REPRESENTATION_CONTEXT(3)
GLOBAL_UNCERTAINTY_ASSIGNED_CONTEXT((#13163))
GLOBAL_UNIT_ASSIGNED_CONTEXT((#13200,#13202,#13203))
REPRESENTATION_CONTEXT('','3D')
);
#13190=(
GEOMETRIC_REPRESENTATION_CONTEXT(3)
GLOBAL_UNCERTAINTY_ASSIGNED_CONTEXT((#13164))
GLOBAL_UNIT_ASSIGNED_CONTEXT((#13200,#13202,#13203))
REPRESENTATION_CONTEXT('','3D')
);
#13191=(
GEOMETRIC_REPRESENTATION_CONTEXT(3)
GLOBAL_UNCERTAINTY_ASSIGNED_CONTEXT((#13165))
GLOBAL_UNIT_ASSIGNED_CONTEXT((#13200,#13202,#13203))
REPRESENTATION_CONTEXT('','3D')
);
#13192=(
GEOMETRIC_REPRESENTATION_CONTEXT(3)
GLOBAL_UNCERTAINTY_ASSIGNED_CONTEXT((#13166))
GLOBAL_UNIT_ASSIGNED_CONTEXT((#13200,#13202,#13203))
REPRESENTATION_CONTEXT('','3D')
);
#13193=(
GEOMETRIC_REPRESENTATION_CONTEXT(3)
GLOBAL_UNCERTAINTY_ASSIGNED_CONTEXT((#13167))
GLOBAL_UNIT_ASSIGNED_CONTEXT((#13200,#13202,#13203))
REPRESENTATION_CONTEXT('','3D')
);
#13194=(
GEOMETRIC_REPRESENTATION_CONTEXT(3)
GLOBAL_UNCERTAINTY_ASSIGNED_CONTEXT((#13168))
GLOBAL_UNIT_ASSIGNED_CONTEXT((#13200,#13202,#13203))
REPRESENTATION_CONTEXT('','3D')
);
#13195=(
GEOMETRIC_REPRESENTATION_CONTEXT(3)
GLOBAL_UNCERTAINTY_ASSIGNED_CONTEXT((#13169))
GLOBAL_UNIT_ASSIGNED_CONTEXT((#13200,#13202,#13203))
REPRESENTATION_CONTEXT('','3D')
);
#13196=(
GEOMETRIC_REPRESENTATION_CONTEXT(3)
GLOBAL_UNCERTAINTY_ASSIGNED_CONTEXT((#13170))
GLOBAL_UNIT_ASSIGNED_CONTEXT((#13200,#13202,#13203))
REPRESENTATION_CONTEXT('','3D')
);
#13197=(
GEOMETRIC_REPRESENTATION_CONTEXT(3)
GLOBAL_UNCERTAINTY_ASSIGNED_CONTEXT((#13171))
GLOBAL_UNIT_ASSIGNED_CONTEXT((#13200,#13202,#13203))
REPRESENTATION_CONTEXT('','3D')
);
#13198=(
GEOMETRIC_REPRESENTATION_CONTEXT(3)
GLOBAL_UNCERTAINTY_ASSIGNED_CONTEXT((#13172))
GLOBAL_UNIT_ASSIGNED_CONTEXT((#13200,#13202,#13203))
REPRESENTATION_CONTEXT('','3D')
);
#13199=(
GEOMETRIC_REPRESENTATION_CONTEXT(3)
GLOBAL_UNCERTAINTY_ASSIGNED_CONTEXT((#13173))
GLOBAL_UNIT_ASSIGNED_CONTEXT((#13200,#13202,#13203))
REPRESENTATION_CONTEXT('','3D')
);
#13200=(
LENGTH_UNIT()
NAMED_UNIT(*)
SI_UNIT(.MILLI.,.METRE.)
);
#13201=(
LENGTH_UNIT()
NAMED_UNIT(*)
SI_UNIT($,.METRE.)
);
#13202=(
NAMED_UNIT(*)
PLANE_ANGLE_UNIT()
SI_UNIT($,.RADIAN.)
);
#13203=(
NAMED_UNIT(*)
SI_UNIT($,.STERADIAN.)
SOLID_ANGLE_UNIT()
);
#13204=SHAPE_DEFINITION_REPRESENTATION(#13229,#13278);
#13205=SHAPE_DEFINITION_REPRESENTATION(#13230,#13279);
#13206=SHAPE_DEFINITION_REPRESENTATION(#13231,#13280);
#13207=SHAPE_DEFINITION_REPRESENTATION(#13232,#13281);
#13208=SHAPE_DEFINITION_REPRESENTATION(#13233,#13282);
#13209=SHAPE_DEFINITION_REPRESENTATION(#13234,#13283);
#13210=SHAPE_DEFINITION_REPRESENTATION(#13235,#13284);
#13211=SHAPE_DEFINITION_REPRESENTATION(#13236,#13285);
#13212=SHAPE_DEFINITION_REPRESENTATION(#13237,#13286);
#13213=SHAPE_DEFINITION_REPRESENTATION(#13240,#13287);
#13214=SHAPE_DEFINITION_REPRESENTATION(#13241,#13288);
#13215=SHAPE_DEFINITION_REPRESENTATION(#13242,#13289);
#13216=SHAPE_DEFINITION_REPRESENTATION(#13245,#13290);
#13217=SHAPE_DEFINITION_REPRESENTATION(#13246,#13291);
#13218=SHAPE_DEFINITION_REPRESENTATION(#13247,#13292);
#13219=SHAPE_DEFINITION_REPRESENTATION(#13248,#13293);
#13220=SHAPE_DEFINITION_REPRESENTATION(#13252,#13294);
#13221=SHAPE_DEFINITION_REPRESENTATION(#13260,#13295);
#13222=SHAPE_DEFINITION_REPRESENTATION(#13261,#13296);
#13223=SHAPE_DEFINITION_REPRESENTATION(#13262,#13297);
#13224=SHAPE_DEFINITION_REPRESENTATION(#13263,#13298);
#13225=SHAPE_DEFINITION_REPRESENTATION(#13264,#13299);
#13226=SHAPE_DEFINITION_REPRESENTATION(#13265,#13300);
#13227=SHAPE_DEFINITION_REPRESENTATION(#13266,#13301);
#13228=SHAPE_DEFINITION_REPRESENTATION(#13267,#13302);
#13229=PRODUCT_DEFINITION_SHAPE('',$,#13304);
#13230=PRODUCT_DEFINITION_SHAPE('',$,#13305);
#13231=PRODUCT_DEFINITION_SHAPE('',$,#13306);
#13232=PRODUCT_DEFINITION_SHAPE('',$,#13307);
#13233=PRODUCT_DEFINITION_SHAPE('',$,#13308);
#13234=PRODUCT_DEFINITION_SHAPE('',$,#13309);
#13235=PRODUCT_DEFINITION_SHAPE('',$,#13310);
#13236=PRODUCT_DEFINITION_SHAPE('',$,#13311);
#13237=PRODUCT_DEFINITION_SHAPE('',$,#13312);
#13238=PRODUCT_DEFINITION_SHAPE($,$,#93);
#13239=PRODUCT_DEFINITION_SHAPE($,$,#94);
#13240=PRODUCT_DEFINITION_SHAPE('',$,#13313);
#13241=PRODUCT_DEFINITION_SHAPE('',$,#13314);
#13242=PRODUCT_DEFINITION_SHAPE('',$,#13315);
#13243=PRODUCT_DEFINITION_SHAPE($,$,#95);
#13244=PRODUCT_DEFINITION_SHAPE($,$,#96);
#13245=PRODUCT_DEFINITION_SHAPE('',$,#13316);
#13246=PRODUCT_DEFINITION_SHAPE('',$,#13317);
#13247=PRODUCT_DEFINITION_SHAPE('',$,#13318);
#13248=PRODUCT_DEFINITION_SHAPE('',$,#13319);
#13249=PRODUCT_DEFINITION_SHAPE($,$,#97);
#13250=PRODUCT_DEFINITION_SHAPE($,$,#98);
#13251=PRODUCT_DEFINITION_SHAPE($,$,#99);
#13252=PRODUCT_DEFINITION_SHAPE('',$,#13320);
#13253=PRODUCT_DEFINITION_SHAPE($,$,#100);
#13254=PRODUCT_DEFINITION_SHAPE($,$,#101);
#13255=PRODUCT_DEFINITION_SHAPE($,$,#102);
#13256=PRODUCT_DEFINITION_SHAPE($,$,#103);
#13257=PRODUCT_DEFINITION_SHAPE($,$,#104);
#13258=PRODUCT_DEFINITION_SHAPE($,$,#105);
#13259=PRODUCT_DEFINITION_SHAPE($,$,#106);
#13260=PRODUCT_DEFINITION_SHAPE('',$,#13321);
#13261=PRODUCT_DEFINITION_SHAPE('',$,#13322);
#13262=PRODUCT_DEFINITION_SHAPE('',$,#13323);
#13263=PRODUCT_DEFINITION_SHAPE('',$,#13324);
#13264=PRODUCT_DEFINITION_SHAPE('',$,#13325);
#13265=PRODUCT_DEFINITION_SHAPE('',$,#13326);
#13266=PRODUCT_DEFINITION_SHAPE('',$,#13327);
#13267=PRODUCT_DEFINITION_SHAPE('',$,#13328);
#13268=PRODUCT_DEFINITION_SHAPE($,$,#107);
#13269=PRODUCT_DEFINITION_SHAPE($,$,#108);
#13270=PRODUCT_DEFINITION_SHAPE($,$,#109);
#13271=PRODUCT_DEFINITION_SHAPE($,$,#110);
#13272=PRODUCT_DEFINITION_SHAPE($,$,#111);
#13273=PRODUCT_DEFINITION_SHAPE($,$,#112);
#13274=PRODUCT_DEFINITION_SHAPE($,$,#113);
#13275=PRODUCT_DEFINITION_SHAPE($,$,#114);
#13276=PRODUCT_DEFINITION_SHAPE($,$,#115);
#13277=PRODUCT_DEFINITION_SHAPE($,$,#116);
#13278=SHAPE_REPRESENTATION('',(#7060,#7826,#7827,#7828),#13174);
#13279=SHAPE_REPRESENTATION('',(#7061),#13175);
#13280=SHAPE_REPRESENTATION('',(#7192,#7610,#7611,#7612,#7613,#7614,#7615,
#7616),#13176);
#13281=SHAPE_REPRESENTATION('',(#7193),#13177);
#13282=SHAPE_REPRESENTATION('',(#7274),#13178);
#13283=SHAPE_REPRESENTATION('',(#7359),#13179);
#13284=SHAPE_REPRESENTATION('',(#7453,#7490,#7491),#13180);
#13285=SHAPE_REPRESENTATION('',(#7454),#13181);
#13286=SHAPE_REPRESENTATION('',(#7474),#13182);
#13287=SHAPE_REPRESENTATION('',(#7492,#7529,#7530),#13183);
#13288=SHAPE_REPRESENTATION('',(#7493),#13184);
#13289=SHAPE_REPRESENTATION('',(#7513),#13185);
#13290=SHAPE_REPRESENTATION('',(#7531,#7592,#7593,#7594),#13186);
#13291=SHAPE_REPRESENTATION('',(#7532),#13187);
#13292=SHAPE_REPRESENTATION('',(#7552),#13188);
#13293=SHAPE_REPRESENTATION('',(#7568),#13189);
#13294=SHAPE_REPRESENTATION('',(#7595),#13190);
#13295=SHAPE_REPRESENTATION('',(#7617,#7821,#7822,#7823,#7824,#7825),#13191);
#13296=SHAPE_REPRESENTATION('',(#7618),#13192);
#13297=SHAPE_REPRESENTATION('',(#7666),#13193);
#13298=SHAPE_REPRESENTATION('',(#7700),#13194);
#13299=SHAPE_REPRESENTATION('',(#7776),#13195);
#13300=SHAPE_REPRESENTATION('',(#7782,#7819,#7820),#13196);
#13301=SHAPE_REPRESENTATION('',(#7783),#13197);
#13302=SHAPE_REPRESENTATION('',(#7803),#13198);
#13303=PRODUCT_DEFINITION_CONTEXT('part definition',#13380,'design');
#13304=PRODUCT_DEFINITION('MAT-041','MAT-041',#13329,#13303);
#13305=PRODUCT_DEFINITION('Base','Base',#13330,#13303);
#13306=PRODUCT_DEFINITION('Index Finger','Index Finger',#13331,#13303);
#13307=PRODUCT_DEFINITION('Finger Link 1','Finger Link 1',#13332,#13303);
#13308=PRODUCT_DEFINITION('Finger Link 2','Finger Link 2',#13333,#13303);
#13309=PRODUCT_DEFINITION('Finger Link 3','Finger Link 3',#13334,#13303);
#13310=PRODUCT_DEFINITION('Pneumatic Actuator 2','Pneumatic Actuator 2',
#13335,#13303);
#13311=PRODUCT_DEFINITION('Actuator 2 Cylinder','Actuator 2 Cylinder',#13336,
#13303);
#13312=PRODUCT_DEFINITION('Actuator 2 Piston Rod',
'Actuator 2 Piston Rod',#13337,#13303);
#13313=PRODUCT_DEFINITION('Pneumatic Actuator 3','Pneumatic Actuator 3',
#13338,#13303);
#13314=PRODUCT_DEFINITION('Actuator 3 Cylinder','Actuator 3 Cylinder',#13339,
#13303);
#13315=PRODUCT_DEFINITION('Actuator 3 Piston Rod',
'Actuator 3 Piston Rod',#13340,#13303);
#13316=PRODUCT_DEFINITION('Pneumatic Actuator 1','Pneumatic Actuator 1',
#13341,#13303);
#13317=PRODUCT_DEFINITION('Actuator 1 Cylinder','Actuator 1 Cylinder',#13342,
#13303);
#13318=PRODUCT_DEFINITION('Actuator 1 Piston Rod',
'Actuator 1 Piston Rod',#13343,#13303);
#13319=PRODUCT_DEFINITION('Actuator 1 Holder','Actuator 1 Holder',#13344,
#13303);
#13320=PRODUCT_DEFINITION('Finger Tip','Finger Tip',#13345,#13303);
#13321=PRODUCT_DEFINITION('Thumb','Thumb',#13346,#13303);
#13322=PRODUCT_DEFINITION('Thumb Joint','Thumb Joint',#13347,#13303);
#13323=PRODUCT_DEFINITION('Thumb Link 1','Thumb Link 1',#13348,#13303);
#13324=PRODUCT_DEFINITION('Thumb Link 2','Thumb Link 2',#13349,#13303);
#13325=PRODUCT_DEFINITION('Thumb Tip','Thumb Tip',#13350,#13303);
#13326=PRODUCT_DEFINITION('Pneumatic Actuator 4','Pneumatic Actuator 4',
#13351,#13303);
#13327=PRODUCT_DEFINITION('Actuator 4 Cylinder','Actuator 4 Cylinder',#13352,
#13303);
#13328=PRODUCT_DEFINITION('Actuator 4 Piston Rod',
'Actuator 4 Piston Rod',#13353,#13303);
#13329=PRODUCT_DEFINITION_FORMATION('',$,#13382);
#13330=PRODUCT_DEFINITION_FORMATION('',$,#13383);
#13331=PRODUCT_DEFINITION_FORMATION('',$,#13384);
#13332=PRODUCT_DEFINITION_FORMATION('',$,#13385);
#13333=PRODUCT_DEFINITION_FORMATION('',$,#13386);
#13334=PRODUCT_DEFINITION_FORMATION('',$,#13387);
#13335=PRODUCT_DEFINITION_FORMATION('',$,#13388);
#13336=PRODUCT_DEFINITION_FORMATION('',$,#13389);
#13337=PRODUCT_DEFINITION_FORMATION('',$,#13390);
#13338=PRODUCT_DEFINITION_FORMATION('',$,#13391);
#13339=PRODUCT_DEFINITION_FORMATION('',$,#13392);
#13340=PRODUCT_DEFINITION_FORMATION('',$,#13393);
#13341=PRODUCT_DEFINITION_FORMATION('',$,#13394);
#13342=PRODUCT_DEFINITION_FORMATION('',$,#13395);
#13343=PRODUCT_DEFINITION_FORMATION('',$,#13396);
#13344=PRODUCT_DEFINITION_FORMATION('',$,#13397);
#13345=PRODUCT_DEFINITION_FORMATION('',$,#13398);
#13346=PRODUCT_DEFINITION_FORMATION('',$,#13399);
#13347=PRODUCT_DEFINITION_FORMATION('',$,#13400);
#13348=PRODUCT_DEFINITION_FORMATION('',$,#13401);
#13349=PRODUCT_DEFINITION_FORMATION('',$,#13402);
#13350=PRODUCT_DEFINITION_FORMATION('',$,#13403);
#13351=PRODUCT_DEFINITION_FORMATION('',$,#13404);
#13352=PRODUCT_DEFINITION_FORMATION('',$,#13405);
#13353=PRODUCT_DEFINITION_FORMATION('',$,#13406);
#13354=PRODUCT_RELATED_PRODUCT_CATEGORY('MAT-041','MAT-041',(#13382));
#13355=PRODUCT_RELATED_PRODUCT_CATEGORY('Base','Base',(#13383));
#13356=PRODUCT_RELATED_PRODUCT_CATEGORY('Index Finger','Index Finger',(#13384));
#13357=PRODUCT_RELATED_PRODUCT_CATEGORY('Finger Link 1','Finger Link 1',
(#13385));
#13358=PRODUCT_RELATED_PRODUCT_CATEGORY('Finger Link 2','Finger Link 2',
(#13386));
#13359=PRODUCT_RELATED_PRODUCT_CATEGORY('Finger Link 3','Finger Link 3',
(#13387));
#13360=PRODUCT_RELATED_PRODUCT_CATEGORY('Pneumatic Actuator 2',
'Pneumatic Actuator 2',(#13388));
#13361=PRODUCT_RELATED_PRODUCT_CATEGORY('Actuator 2 Cylinder',
'Actuator 2 Cylinder',(#13389));
#13362=PRODUCT_RELATED_PRODUCT_CATEGORY('Actuator 2 Piston Rod',
'Actuator 2 Piston Rod',(#13390));
#13363=PRODUCT_RELATED_PRODUCT_CATEGORY('Pneumatic Actuator 3',
'Pneumatic Actuator 3',(#13391));
#13364=PRODUCT_RELATED_PRODUCT_CATEGORY('Actuator 3 Cylinder',
'Actuator 3 Cylinder',(#13392));
#13365=PRODUCT_RELATED_PRODUCT_CATEGORY('Actuator 3 Piston Rod',
'Actuator 3 Piston Rod',(#13393));
#13366=PRODUCT_RELATED_PRODUCT_CATEGORY('Pneumatic Actuator 1',
'Pneumatic Actuator 1',(#13394));
#13367=PRODUCT_RELATED_PRODUCT_CATEGORY('Actuator 1 Cylinder',
'Actuator 1 Cylinder',(#13395));
#13368=PRODUCT_RELATED_PRODUCT_CATEGORY('Actuator 1 Piston Rod',
'Actuator 1 Piston Rod',(#13396));
#13369=PRODUCT_RELATED_PRODUCT_CATEGORY('Actuator 1 Holder',
'Actuator 1 Holder',(#13397));
#13370=PRODUCT_RELATED_PRODUCT_CATEGORY('Finger Tip','Finger Tip',(#13398));
#13371=PRODUCT_RELATED_PRODUCT_CATEGORY('Thumb','Thumb',(#13399));
#13372=PRODUCT_RELATED_PRODUCT_CATEGORY('Thumb Joint','Thumb Joint',(#13400));
#13373=PRODUCT_RELATED_PRODUCT_CATEGORY('Thumb Link 1','Thumb Link 1',(#13401));
#13374=PRODUCT_RELATED_PRODUCT_CATEGORY('Thumb Link 2','Thumb Link 2',(#13402));
#13375=PRODUCT_RELATED_PRODUCT_CATEGORY('Thumb Tip','Thumb Tip',(#13403));
#13376=PRODUCT_RELATED_PRODUCT_CATEGORY('Pneumatic Actuator 4',
'Pneumatic Actuator 4',(#13404));
#13377=PRODUCT_RELATED_PRODUCT_CATEGORY('Actuator 4 Cylinder',
'Actuator 4 Cylinder',(#13405));
#13378=PRODUCT_RELATED_PRODUCT_CATEGORY('Actuator 4 Piston Rod',
'Actuator 4 Piston Rod',(#13406));
#13379=APPLICATION_PROTOCOL_DEFINITION('international standard',
'automotive_design',2009,#13380);
#13380=APPLICATION_CONTEXT(
'Core Data for Automotive Mechanical Design Process');
#13381=PRODUCT_CONTEXT('part definition',#13380,'mechanical');
#13382=PRODUCT('MAT-041','MAT-041','STEP AP214',(#13381));
#13383=PRODUCT('Base','Base','Base',(#13381));
#13384=PRODUCT('Index Finger','Index Finger',$,(#13381));
#13385=PRODUCT('Finger Link 1','Finger Link 1',$,(#13381));
#13386=PRODUCT('Finger Link 2','Finger Link 2',$,(#13381));
#13387=PRODUCT('Finger Link 3','Finger Link 3',$,(#13381));
#13388=PRODUCT('Pneumatic Actuator 2','Pneumatic Actuator 2',$,(#13381));
#13389=PRODUCT('Actuator 2 Cylinder','Actuator 2 Cylinder',$,(#13381));
#13390=PRODUCT('Actuator 2 Piston Rod','Actuator 2 Piston Rod',$,(#13381));
#13391=PRODUCT('Pneumatic Actuator 3','Pneumatic Actuator 3',$,(#13381));
#13392=PRODUCT('Actuator 3 Cylinder','Actuator 3 Cylinder',$,(#13381));
#13393=PRODUCT('Actuator 3 Piston Rod','Actuator 3 Piston Rod',$,(#13381));
#13394=PRODUCT('Pneumatic Actuator 1','Pneumatic Actuator 1',$,(#13381));
#13395=PRODUCT('Actuator 1 Cylinder','Actuator 1 Cylinder',$,(#13381));
#13396=PRODUCT('Actuator 1 Piston Rod','Actuator 1 Piston Rod',$,(#13381));
#13397=PRODUCT('Actuator 1 Holder','Actuator 1 Holder',$,(#13381));
#13398=PRODUCT('Finger Tip','Finger Tip',$,(#13381));
#13399=PRODUCT('Thumb','Thumb',$,(#13381));
#13400=PRODUCT('Thumb Joint','Thumb Joint',$,(#13381));
#13401=PRODUCT('Thumb Link 1','Thumb Link 1',$,(#13381));
#13402=PRODUCT('Thumb Link 2','Thumb Link 2',$,(#13381));
#13403=PRODUCT('Thumb Tip','Thumb Tip',$,(#13381));
#13404=PRODUCT('Pneumatic Actuator 4','Pneumatic Actuator 4',$,(#13381));
#13405=PRODUCT('Actuator 4 Cylinder','Actuator 4 Cylinder',$,(#13381));
#13406=PRODUCT('Actuator 4 Piston Rod','Actuator 4 Piston Rod',$,(#13381));
#13407=PRESENTATION_STYLE_ASSIGNMENT((#13412));
#13408=PRESENTATION_STYLE_ASSIGNMENT((#13413));
#13409=PRESENTATION_STYLE_ASSIGNMENT((#13414));
#13410=PRESENTATION_STYLE_ASSIGNMENT((#13415));
#13411=PRESENTATION_STYLE_ASSIGNMENT((#13416));
#13412=SURFACE_STYLE_USAGE(.BOTH.,#13417);
#13413=SURFACE_STYLE_USAGE(.BOTH.,#13418);
#13414=SURFACE_STYLE_USAGE(.BOTH.,#13419);
#13415=SURFACE_STYLE_USAGE(.BOTH.,#13420);
#13416=SURFACE_STYLE_USAGE(.BOTH.,#13421);
#13417=SURFACE_SIDE_STYLE('',(#13422));
#13418=SURFACE_SIDE_STYLE('',(#13423));
#13419=SURFACE_SIDE_STYLE('',(#13424));
#13420=SURFACE_SIDE_STYLE('',(#13425));
#13421=SURFACE_SIDE_STYLE('',(#13426));
#13422=SURFACE_STYLE_FILL_AREA(#13427);
#13423=SURFACE_STYLE_FILL_AREA(#13428);
#13424=SURFACE_STYLE_FILL_AREA(#13429);
#13425=SURFACE_STYLE_FILL_AREA(#13430);
#13426=SURFACE_STYLE_FILL_AREA(#13431);
#13427=FILL_AREA_STYLE('Steel - Satin',(#13432));
#13428=FILL_AREA_STYLE('Opaque(20,51,87)',(#13433));
#13429=FILL_AREA_STYLE('Opaque(61,176,222)',(#13434));
#13430=FILL_AREA_STYLE('Opaque(227,224,212)',(#13435));
#13431=FILL_AREA_STYLE('Opaque(97,158,199)',(#13436));
#13432=FILL_AREA_STYLE_COLOUR('Steel - Satin',#13437);
#13433=FILL_AREA_STYLE_COLOUR('Opaque(20,51,87)',#13438);
#13434=FILL_AREA_STYLE_COLOUR('Opaque(61,176,222)',#13439);
#13435=FILL_AREA_STYLE_COLOUR('Opaque(227,224,212)',#13440);
#13436=FILL_AREA_STYLE_COLOUR('Opaque(97,158,199)',#13441);
#13437=COLOUR_RGB('Steel - Satin',0.627450980392157,0.627450980392157,0.627450980392157);
#13438=COLOUR_RGB('Opaque(20,51,87)',0.0784313725490196,0.2,0.341176470588235);
#13439=COLOUR_RGB('Opaque(61,176,222)',0.23921568627451,0.690196078431373,
0.870588235294118);
#13440=COLOUR_RGB('Opaque(227,224,212)',0.890196078431372,0.87843137254902,
0.831372549019608);
#13441=COLOUR_RGB('Opaque(97,158,199)',0.380392156862745,0.619607843137255,
0.780392156862745);
ENDSEC;
END-ISO-10303-21;
